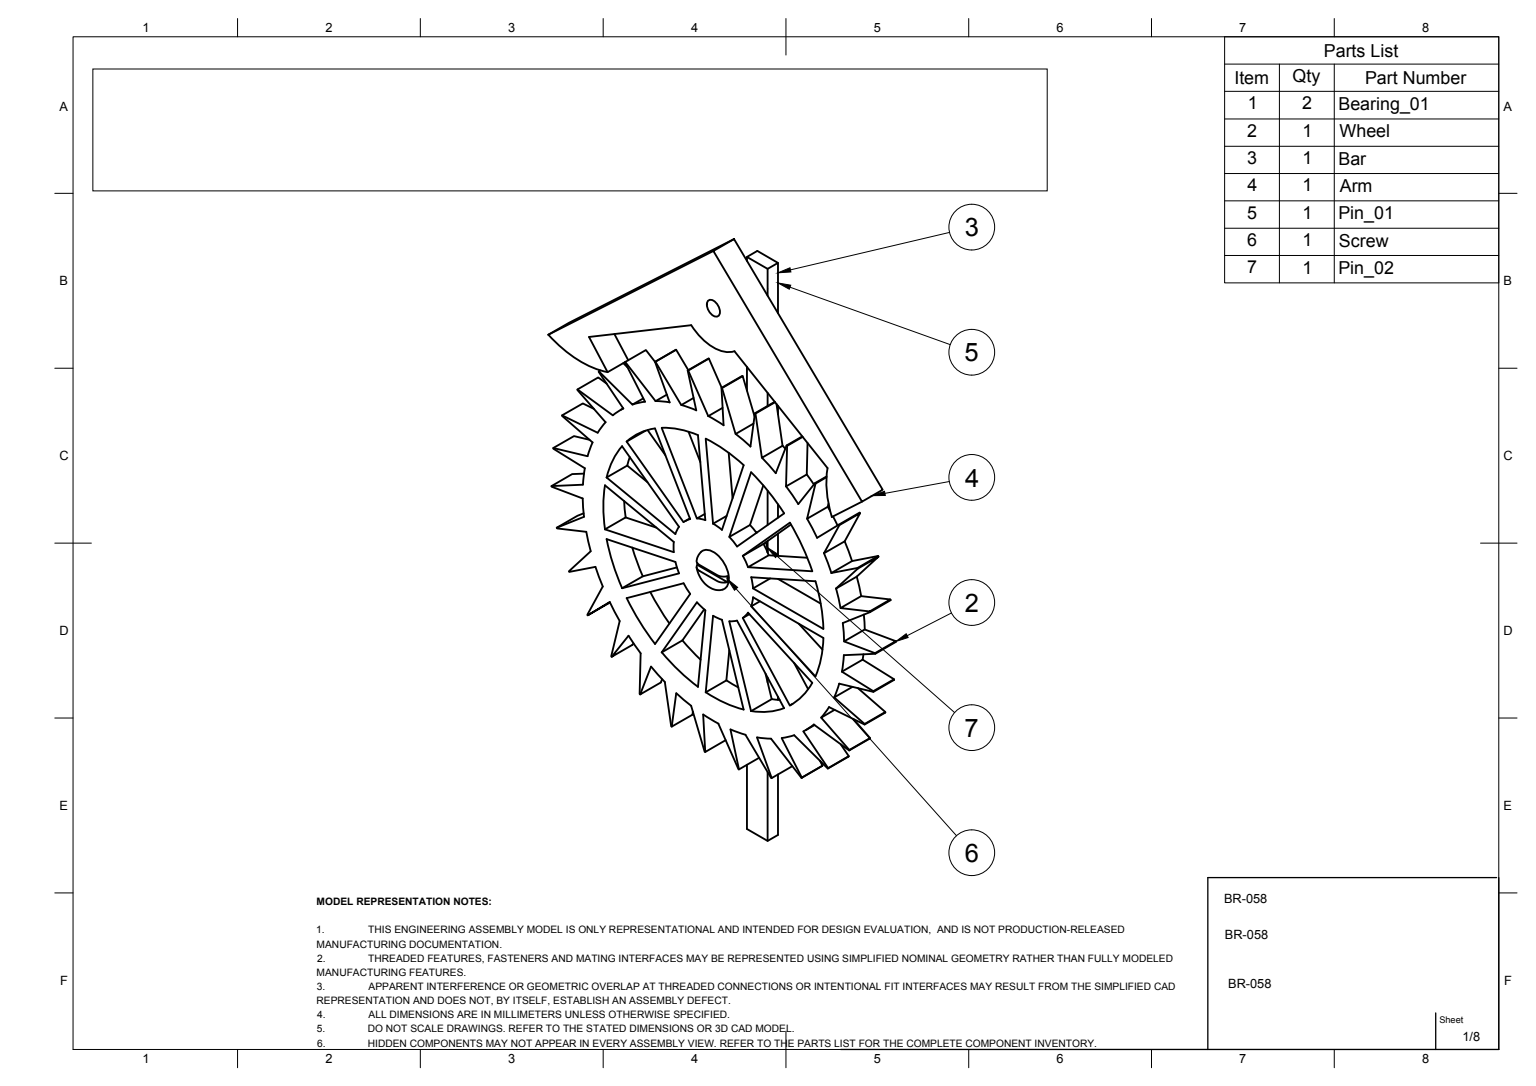
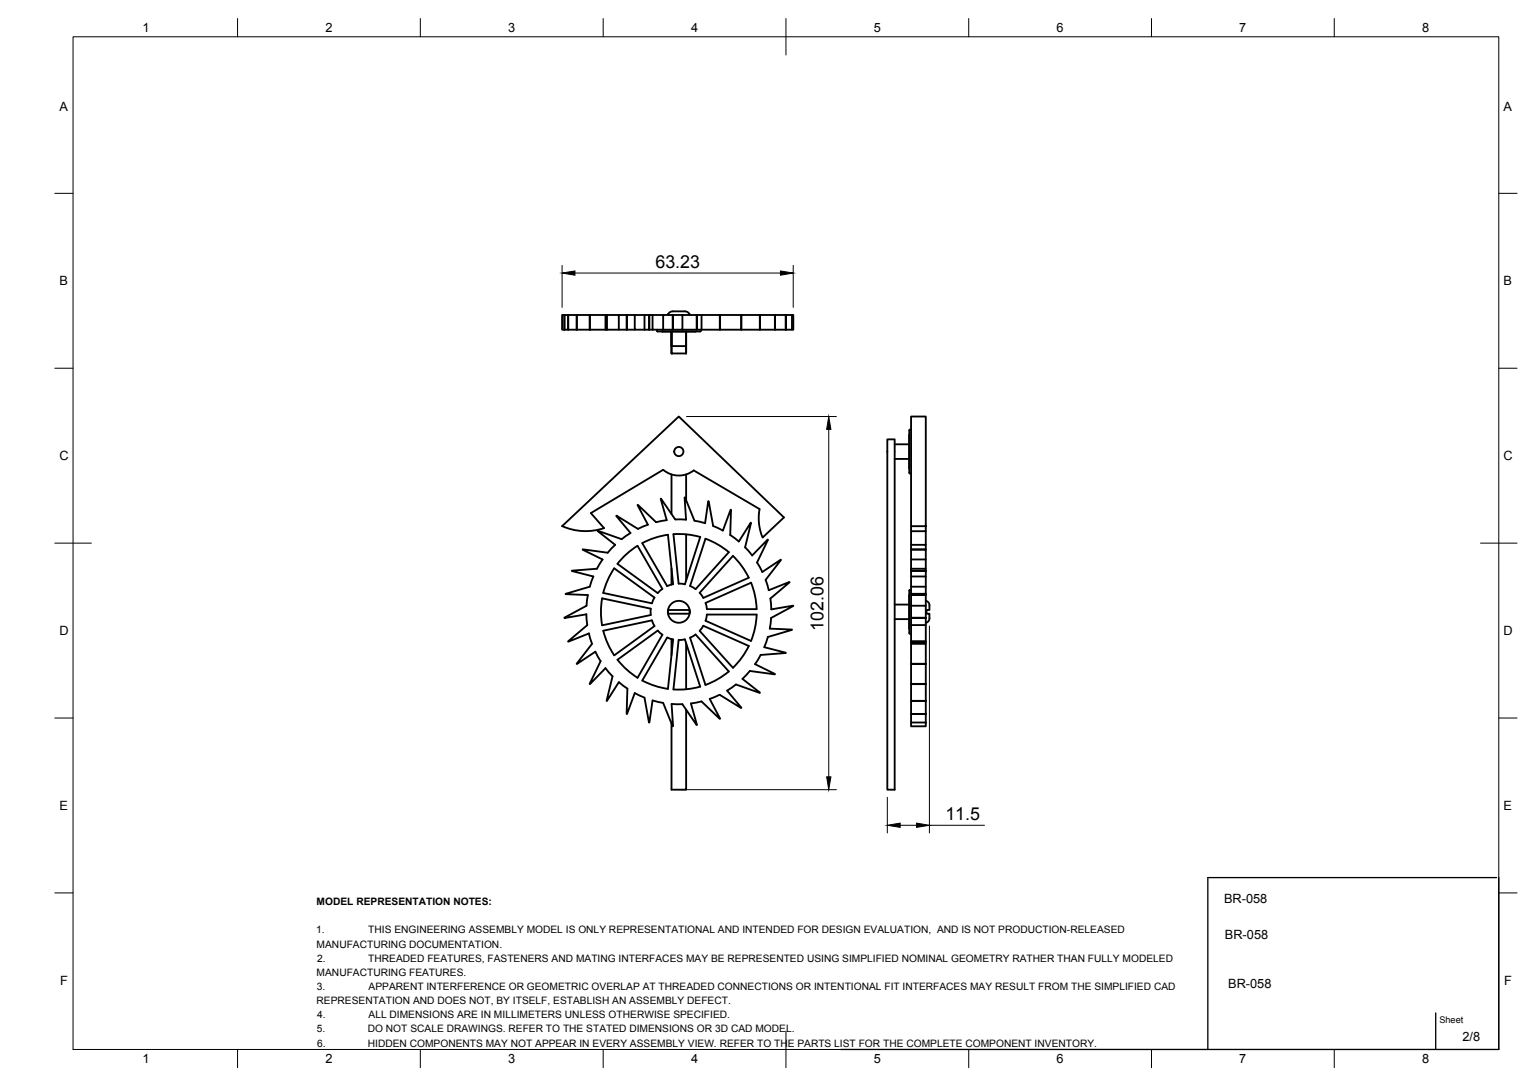
ISO-10303-21;
HEADER;
/* Generated by software containing ST-Developer
 * from STEP Tools, Inc. (www.steptools.com) 
 */

FILE_DESCRIPTION(
/* description */ (''),
/* implementation_level */ '2;1');

FILE_NAME(
/* name */ 'BR-058',
/* time_stamp */ '2026-10-12T16:07:47-07:00',
/* author */ (''),
/* organization */ (''),
/* preprocessor_version */ 'ST-DEVELOPER v20.2',
/* originating_system */ 'Autodesk Translation Framework v15.15.0.0',
/* authorisation */ '');

FILE_SCHEMA (('AUTOMOTIVE_DESIGN { 1 0 10303 214 3 1 1 }'));
ENDSEC;

DATA;
#10=MECHANICAL_DESIGN_GEOMETRIC_PRESENTATION_REPRESENTATION('',(#94,#95,
#96,#97,#98,#99,#100,#101,#102,#103),#8779);
#11=ITEM_DEFINED_TRANSFORMATION($,$,#5571,#5714);
#12=ITEM_DEFINED_TRANSFORMATION($,$,#5203,#5715);
#13=ITEM_DEFINED_TRANSFORMATION($,$,#5509,#5716);
#14=ITEM_DEFINED_TRANSFORMATION($,$,#5519,#5717);
#15=ITEM_DEFINED_TRANSFORMATION($,$,#5540,#5718);
#16=ITEM_DEFINED_TRANSFORMATION($,$,#5546,#5719);
#17=ITEM_DEFINED_TRANSFORMATION($,$,#5565,#5720);
#18=ITEM_DEFINED_TRANSFORMATION($,$,#5571,#5721);
#19=(
REPRESENTATION_RELATIONSHIP($,$,#8815,#8808)
REPRESENTATION_RELATIONSHIP_WITH_TRANSFORMATION(#11)
SHAPE_REPRESENTATION_RELATIONSHIP()
);
#20=(
REPRESENTATION_RELATIONSHIP($,$,#8809,#8808)
REPRESENTATION_RELATIONSHIP_WITH_TRANSFORMATION(#12)
SHAPE_REPRESENTATION_RELATIONSHIP()
);
#21=(
REPRESENTATION_RELATIONSHIP($,$,#8810,#8808)
REPRESENTATION_RELATIONSHIP_WITH_TRANSFORMATION(#13)
SHAPE_REPRESENTATION_RELATIONSHIP()
);
#22=(
REPRESENTATION_RELATIONSHIP($,$,#8811,#8808)
REPRESENTATION_RELATIONSHIP_WITH_TRANSFORMATION(#14)
SHAPE_REPRESENTATION_RELATIONSHIP()
);
#23=(
REPRESENTATION_RELATIONSHIP($,$,#8812,#8808)
REPRESENTATION_RELATIONSHIP_WITH_TRANSFORMATION(#15)
SHAPE_REPRESENTATION_RELATIONSHIP()
);
#24=(
REPRESENTATION_RELATIONSHIP($,$,#8813,#8808)
REPRESENTATION_RELATIONSHIP_WITH_TRANSFORMATION(#16)
SHAPE_REPRESENTATION_RELATIONSHIP()
);
#25=(
REPRESENTATION_RELATIONSHIP($,$,#8814,#8808)
REPRESENTATION_RELATIONSHIP_WITH_TRANSFORMATION(#17)
SHAPE_REPRESENTATION_RELATIONSHIP()
);
#26=(
REPRESENTATION_RELATIONSHIP($,$,#8815,#8808)
REPRESENTATION_RELATIONSHIP_WITH_TRANSFORMATION(#18)
SHAPE_REPRESENTATION_RELATIONSHIP()
);
#27=CONTEXT_DEPENDENT_SHAPE_REPRESENTATION(#19,#8800);
#28=CONTEXT_DEPENDENT_SHAPE_REPRESENTATION(#20,#8801);
#29=CONTEXT_DEPENDENT_SHAPE_REPRESENTATION(#21,#8802);
#30=CONTEXT_DEPENDENT_SHAPE_REPRESENTATION(#22,#8803);
#31=CONTEXT_DEPENDENT_SHAPE_REPRESENTATION(#23,#8804);
#32=CONTEXT_DEPENDENT_SHAPE_REPRESENTATION(#24,#8805);
#33=CONTEXT_DEPENDENT_SHAPE_REPRESENTATION(#25,#8806);
#34=CONTEXT_DEPENDENT_SHAPE_REPRESENTATION(#26,#8807);
#35=NEXT_ASSEMBLY_USAGE_OCCURRENCE('Bearing_01:1','Bearing_01:1',
'Bearing_01:1',#8817,#8824,'Bearing_01:1');
#36=NEXT_ASSEMBLY_USAGE_OCCURRENCE('Wheel:1','Wheel:1','Wheel:1',#8817,
#8818,'Wheel:1');
#37=NEXT_ASSEMBLY_USAGE_OCCURRENCE('Bar:1','Bar:1','Bar:1',#8817,#8819,
'Bar:1');
#38=NEXT_ASSEMBLY_USAGE_OCCURRENCE('Arm:1','Arm:1','Arm:1',#8817,#8820,
'Arm:1');
#39=NEXT_ASSEMBLY_USAGE_OCCURRENCE('Pin_01:1','Pin_01:1','Pin_01:1',#8817,
#8821,'Pin_01:1');
#40=NEXT_ASSEMBLY_USAGE_OCCURRENCE('Screw:1','Screw:1','Screw:1',#8817,
#8822,'Screw:1');
#41=NEXT_ASSEMBLY_USAGE_OCCURRENCE('Pin_02:1','Pin_02:1','Pin_02:1',#8817,
#8823,'Pin_02:1');
#42=NEXT_ASSEMBLY_USAGE_OCCURRENCE('Bearing_01:2','Bearing_01:2',
'Bearing_01:2',#8817,#8824,'Bearing_01:2');
#43=CONICAL_SURFACE('',#5582,4.8,0.785398163397444);
#44=CONICAL_SURFACE('',#5593,4.845,0.785398163397444);
#45=CONICAL_SURFACE('',#5599,3.1184375,0.785398163397448);
#46=CONICAL_SURFACE('',#5617,3.0734375,0.785398163397448);
#47=CONICAL_SURFACE('',#5639,4.36638040039984,0.52359877559829);
#48=CONICAL_SURFACE('',#5648,4.57071796769724,1.04719755119659);
#49=CONICAL_SURFACE('',#5657,4.62071796769724,1.04719755119659);
#50=CONICAL_SURFACE('',#5666,4.27977786002139,0.52359877559829);
#51=CONICAL_SURFACE('',#5680,4.36638040039984,0.52359877559829);
#52=CONICAL_SURFACE('',#5689,4.57071796769724,1.04719755119659);
#53=CONICAL_SURFACE('',#5698,4.62071796769724,1.04719755119659);
#54=CONICAL_SURFACE('',#5707,4.27977786002139,0.52359877559829);
#55=TOROIDAL_SURFACE('',#5558,1.77525512860841,1.25);
#56=TOROIDAL_SURFACE('',#5584,5.8,0.2);
#57=TOROIDAL_SURFACE('',#5590,5.8,0.2);
#58=TOROIDAL_SURFACE('',#5605,3.25741379310345,0.138976293103448);
#59=TOROIDAL_SURFACE('',#5611,3.25741379310345,0.138976293103448);
#60=TOROIDAL_SURFACE('',#5619,2.2,0.2);
#61=TOROIDAL_SURFACE('',#5625,2.2,0.2);
#62=TOROIDAL_SURFACE('',#5635,4.14313829631318,0.0900000000000005);
#63=TOROIDAL_SURFACE('',#5641,4.38370090847553,0.0200000000000002);
#64=TOROIDAL_SURFACE('',#5644,4.58,0.119999999999999);
#65=TOROIDAL_SURFACE('',#5650,4.51071796769724,0.12);
#66=TOROIDAL_SURFACE('',#5653,4.51071796769724,0.22);
#67=TOROIDAL_SURFACE('',#5659,4.58,0.219999999999999);
#68=TOROIDAL_SURFACE('',#5662,4.38370090847553,0.12);
#69=TOROIDAL_SURFACE('',#5676,4.14313829631318,0.0900000000000005);
#70=TOROIDAL_SURFACE('',#5682,4.38370090847553,0.0200000000000002);
#71=TOROIDAL_SURFACE('',#5685,4.58,0.119999999999999);
#72=TOROIDAL_SURFACE('',#5691,4.51071796769724,0.12);
#73=TOROIDAL_SURFACE('',#5694,4.51071796769724,0.22);
#74=TOROIDAL_SURFACE('',#5700,4.58,0.219999999999999);
#75=TOROIDAL_SURFACE('',#5703,4.38370090847553,0.12);
#76=B_SPLINE_CURVE_WITH_KNOTS('',3,(#8451,#8452,#8453,#8454,#8455,#8456,
#8457,#8458,#8459,#8460),.UNSPECIFIED.,.F.,.F.,(4,2,2,2,4),(0.042485066523561,
0.0459790210316649,0.0922828710125633,0.139235462221755,0.187535404261205),
 .UNSPECIFIED.);
#77=B_SPLINE_CURVE_WITH_KNOTS('',3,(#8464,#8465,#8466,#8467,#8468,#8469,
#8470,#8471,#8472,#8473),.UNSPECIFIED.,.F.,.F.,(4,2,2,2,4),(0.589058059380764,
0.637358001420214,0.684310592629405,0.730614442610304,0.734108397118407),
 .UNSPECIFIED.);
#78=B_SPLINE_CURVE_WITH_KNOTS('',3,(#8485,#8486,#8487,#8488,#8489,#8490,
#8491,#8492,#8493,#8494),.UNSPECIFIED.,.F.,.F.,(4,2,2,2,4),(0.589058059380764,
0.637358001420214,0.684310592629405,0.730614442610304,0.734108397118408),
 .UNSPECIFIED.);
#79=B_SPLINE_CURVE_WITH_KNOTS('',3,(#8497,#8498,#8499,#8500,#8501,#8502,
#8503,#8504,#8505,#8506),.UNSPECIFIED.,.F.,.F.,(4,2,2,2,4),(0.0424850665235609,
0.0459790210316651,0.0922828710125635,0.139235462221755,0.187535404261205),
 .UNSPECIFIED.);
#80=SHAPE_REPRESENTATION_RELATIONSHIP('SRR','None',#8809,#87);
#81=SHAPE_REPRESENTATION_RELATIONSHIP('SRR','None',#8810,#88);
#82=SHAPE_REPRESENTATION_RELATIONSHIP('SRR','None',#8811,#89);
#83=SHAPE_REPRESENTATION_RELATIONSHIP('SRR','None',#8812,#90);
#84=SHAPE_REPRESENTATION_RELATIONSHIP('SRR','None',#8813,#91);
#85=SHAPE_REPRESENTATION_RELATIONSHIP('SRR','None',#8814,#92);
#86=SHAPE_REPRESENTATION_RELATIONSHIP('SRR','None',#8815,#93);
#87=ADVANCED_BREP_SHAPE_REPRESENTATION('',(#104),#8772);
#88=ADVANCED_BREP_SHAPE_REPRESENTATION('',(#105),#8773);
#89=ADVANCED_BREP_SHAPE_REPRESENTATION('',(#106),#8774);
#90=ADVANCED_BREP_SHAPE_REPRESENTATION('',(#107),#8775);
#91=ADVANCED_BREP_SHAPE_REPRESENTATION('',(#108),#8776);
#92=ADVANCED_BREP_SHAPE_REPRESENTATION('',(#109),#8777);
#93=ADVANCED_BREP_SHAPE_REPRESENTATION('',(#110,#111,#112,#113),#8778);
#94=STYLED_ITEM('',(#8853),#104);
#95=STYLED_ITEM('',(#8854),#105);
#96=STYLED_ITEM('',(#8855),#106);
#97=STYLED_ITEM('',(#8854),#107);
#98=STYLED_ITEM('',(#8856),#108);
#99=STYLED_ITEM('',(#8856),#109);
#100=STYLED_ITEM('',(#8856),#110);
#101=STYLED_ITEM('',(#8856),#111);
#102=STYLED_ITEM('',(#8856),#112);
#103=STYLED_ITEM('',(#8856),#113);
#104=MANIFOLD_SOLID_BREP('Body1',#5114);
#105=MANIFOLD_SOLID_BREP('Body1',#5115);
#106=MANIFOLD_SOLID_BREP('Body1',#5116);
#107=MANIFOLD_SOLID_BREP('Body1',#5117);
#108=MANIFOLD_SOLID_BREP('Body1',#5118);
#109=MANIFOLD_SOLID_BREP('Body1',#5119);
#110=MANIFOLD_SOLID_BREP('Body1',#5120);
#111=MANIFOLD_SOLID_BREP('Body2',#5121);
#112=MANIFOLD_SOLID_BREP('Body3',#5122);
#113=MANIFOLD_SOLID_BREP('Body4',#5123);
#114=FACE_BOUND('',#934,.T.);
#115=FACE_BOUND('',#935,.T.);
#116=FACE_BOUND('',#936,.T.);
#117=FACE_BOUND('',#937,.T.);
#118=FACE_BOUND('',#938,.T.);
#119=FACE_BOUND('',#939,.T.);
#120=FACE_BOUND('',#940,.T.);
#121=FACE_BOUND('',#941,.T.);
#122=FACE_BOUND('',#942,.T.);
#123=FACE_BOUND('',#943,.T.);
#124=FACE_BOUND('',#944,.T.);
#125=FACE_BOUND('',#945,.T.);
#126=FACE_BOUND('',#946,.T.);
#127=FACE_BOUND('',#947,.T.);
#128=FACE_BOUND('',#948,.T.);
#129=FACE_BOUND('',#949,.T.);
#130=FACE_BOUND('',#951,.T.);
#131=FACE_BOUND('',#952,.T.);
#132=FACE_BOUND('',#953,.T.);
#133=FACE_BOUND('',#954,.T.);
#134=FACE_BOUND('',#955,.T.);
#135=FACE_BOUND('',#956,.T.);
#136=FACE_BOUND('',#957,.T.);
#137=FACE_BOUND('',#958,.T.);
#138=FACE_BOUND('',#959,.T.);
#139=FACE_BOUND('',#960,.T.);
#140=FACE_BOUND('',#961,.T.);
#141=FACE_BOUND('',#962,.T.);
#142=FACE_BOUND('',#963,.T.);
#143=FACE_BOUND('',#964,.T.);
#144=FACE_BOUND('',#965,.T.);
#145=FACE_BOUND('',#966,.T.);
#146=FACE_BOUND('',#973,.T.);
#147=FACE_BOUND('',#975,.T.);
#148=FACE_BOUND('',#987,.T.);
#149=FACE_BOUND('',#989,.T.);
#150=FACE_BOUND('',#994,.T.);
#151=FACE_BOUND('',#1015,.T.);
#152=FACE_BOUND('',#1017,.T.);
#153=FACE_BOUND('',#1019,.T.);
#154=FACE_BOUND('',#1021,.T.);
#155=FACE_BOUND('',#1033,.T.);
#156=FACE_BOUND('',#1035,.T.);
#157=FACE_BOUND('',#1037,.T.);
#158=FACE_BOUND('',#1039,.T.);
#159=FACE_BOUND('',#1053,.T.);
#160=FACE_BOUND('',#1055,.T.);
#161=FACE_BOUND('',#1057,.T.);
#162=FACE_BOUND('',#1059,.T.);
#163=FACE_BOUND('',#1061,.T.);
#164=FACE_BOUND('',#1075,.T.);
#165=FACE_BOUND('',#1077,.T.);
#166=FACE_BOUND('',#1079,.T.);
#167=FACE_BOUND('',#1081,.T.);
#168=FACE_BOUND('',#1083,.T.);
#169=CIRCLE('',#5208,25.2882678496568);
#170=CIRCLE('',#5209,25.2882678496568);
#171=CIRCLE('',#5211,25.2882678496568);
#172=CIRCLE('',#5212,25.2882678496568);
#173=CIRCLE('',#5217,25.2882678496568);
#174=CIRCLE('',#5218,25.2882678496568);
#175=CIRCLE('',#5220,25.2882678496568);
#176=CIRCLE('',#5221,25.2882678496568);
#177=CIRCLE('',#5226,25.2882678496568);
#178=CIRCLE('',#5227,25.2882678496568);
#179=CIRCLE('',#5232,25.2882678496568);
#180=CIRCLE('',#5233,25.2882678496568);
#181=CIRCLE('',#5235,25.2882678496568);
#182=CIRCLE('',#5236,25.2882678496568);
#183=CIRCLE('',#5244,25.2882678496568);
#184=CIRCLE('',#5245,25.2882678496568);
#185=CIRCLE('',#5250,25.2882678496568);
#186=CIRCLE('',#5251,25.2882678496568);
#187=CIRCLE('',#5258,21.2882678496568);
#188=CIRCLE('',#5259,21.2882678496568);
#189=CIRCLE('',#5261,21.2882678496568);
#190=CIRCLE('',#5262,21.2882678496568);
#191=CIRCLE('',#5264,7.71108476483471);
#192=CIRCLE('',#5265,7.71108476483471);
#193=CIRCLE('',#5267,7.71108476483471);
#194=CIRCLE('',#5268,7.71108476483471);
#195=CIRCLE('',#5272,21.2882678496568);
#196=CIRCLE('',#5273,21.2882678496568);
#197=CIRCLE('',#5275,7.71108476483471);
#198=CIRCLE('',#5276,7.71108476483471);
#199=CIRCLE('',#5280,21.2882678496568);
#200=CIRCLE('',#5281,21.2882678496568);
#201=CIRCLE('',#5283,7.71108476483471);
#202=CIRCLE('',#5284,7.71108476483471);
#203=CIRCLE('',#5289,25.2882678496568);
#204=CIRCLE('',#5290,25.2882678496568);
#205=CIRCLE('',#5292,25.2882678496568);
#206=CIRCLE('',#5293,25.2882678496568);
#207=CIRCLE('',#5298,25.2882678496568);
#208=CIRCLE('',#5299,25.2882678496568);
#209=CIRCLE('',#5301,25.2882678496568);
#210=CIRCLE('',#5302,25.2882678496568);
#211=CIRCLE('',#5307,25.2882678496568);
#212=CIRCLE('',#5308,25.2882678496568);
#213=CIRCLE('',#5316,25.2882678496568);
#214=CIRCLE('',#5317,25.2882678496568);
#215=CIRCLE('',#5324,21.2882678496568);
#216=CIRCLE('',#5325,21.2882678496568);
#217=CIRCLE('',#5327,21.2882678496568);
#218=CIRCLE('',#5328,21.2882678496568);
#219=CIRCLE('',#5330,7.71108476483471);
#220=CIRCLE('',#5331,7.71108476483471);
#221=CIRCLE('',#5333,7.71108476483471);
#222=CIRCLE('',#5334,7.71108476483471);
#223=CIRCLE('',#5338,21.2882678496568);
#224=CIRCLE('',#5339,21.2882678496568);
#225=CIRCLE('',#5341,7.71108476483471);
#226=CIRCLE('',#5342,7.71108476483471);
#227=CIRCLE('',#5346,21.2882678496568);
#228=CIRCLE('',#5347,21.2882678496568);
#229=CIRCLE('',#5349,21.2882678496568);
#230=CIRCLE('',#5350,21.2882678496568);
#231=CIRCLE('',#5352,7.71108476483471);
#232=CIRCLE('',#5353,7.71108476483471);
#233=CIRCLE('',#5355,7.71108476483471);
#234=CIRCLE('',#5356,7.71108476483471);
#235=CIRCLE('',#5360,21.2882678496568);
#236=CIRCLE('',#5361,21.2882678496568);
#237=CIRCLE('',#5363,21.2882678496568);
#238=CIRCLE('',#5364,21.2882678496568);
#239=CIRCLE('',#5366,7.71108476483471);
#240=CIRCLE('',#5367,7.71108476483471);
#241=CIRCLE('',#5369,7.71108476483471);
#242=CIRCLE('',#5370,7.71108476483471);
#243=CIRCLE('',#5374,21.2882678496568);
#244=CIRCLE('',#5375,21.2882678496568);
#245=CIRCLE('',#5377,7.71108476483471);
#246=CIRCLE('',#5378,7.71108476483471);
#247=CIRCLE('',#5384,21.2882678496568);
#248=CIRCLE('',#5385,21.2882678496568);
#249=CIRCLE('',#5387,7.71108476483471);
#250=CIRCLE('',#5388,7.71108476483471);
#251=CIRCLE('',#5395,25.2882678496568);
#252=CIRCLE('',#5396,25.2882678496568);
#253=CIRCLE('',#5398,25.2882678496568);
#254=CIRCLE('',#5399,25.2882678496568);
#255=CIRCLE('',#5404,25.2882678496568);
#256=CIRCLE('',#5405,25.2882678496568);
#257=CIRCLE('',#5410,25.2882678496568);
#258=CIRCLE('',#5411,25.2882678496568);
#259=CIRCLE('',#5413,25.2882678496568);
#260=CIRCLE('',#5414,25.2882678496568);
#261=CIRCLE('',#5419,25.2882678496568);
#262=CIRCLE('',#5420,25.2882678496568);
#263=CIRCLE('',#5422,25.2882678496568);
#264=CIRCLE('',#5423,25.2882678496568);
#265=CIRCLE('',#5437,25.2882678496568);
#266=CIRCLE('',#5438,25.2882678496568);
#267=CIRCLE('',#5442,21.2882678496568);
#268=CIRCLE('',#5443,21.2882678496568);
#269=CIRCLE('',#5445,7.71108476483471);
#270=CIRCLE('',#5446,7.71108476483471);
#271=CIRCLE('',#5450,21.2882678496568);
#272=CIRCLE('',#5451,21.2882678496568);
#273=CIRCLE('',#5453,7.71108476483471);
#274=CIRCLE('',#5454,7.71108476483471);
#275=CIRCLE('',#5461,25.2882678496568);
#276=CIRCLE('',#5462,25.2882678496568);
#277=CIRCLE('',#5464,25.2882678496568);
#278=CIRCLE('',#5465,25.2882678496568);
#279=CIRCLE('',#5470,25.2882678496568);
#280=CIRCLE('',#5471,25.2882678496568);
#281=CIRCLE('',#5476,25.2882678496568);
#282=CIRCLE('',#5477,25.2882678496568);
#283=CIRCLE('',#5479,25.2882678496568);
#284=CIRCLE('',#5480,25.2882678496568);
#285=CIRCLE('',#5485,25.2882678496568);
#286=CIRCLE('',#5486,25.2882678496568);
#287=CIRCLE('',#5491,25.2882678496568);
#288=CIRCLE('',#5492,25.2882678496568);
#289=CIRCLE('',#5505,1.99137169252308);
#290=CIRCLE('',#5506,1.99137169252308);
#291=CIRCLE('',#5511,1.26938918348039);
#292=CIRCLE('',#5512,1.26938918348039);
#293=CIRCLE('',#5523,6.58030196793658);
#294=CIRCLE('',#5524,6.58030196793658);
#295=CIRCLE('',#5528,1.26938918348039);
#296=CIRCLE('',#5529,1.26938918348039);
#297=CIRCLE('',#5532,13.6540067108022);
#298=CIRCLE('',#5533,13.6540067108022);
#299=CIRCLE('',#5536,15.694333954976);
#300=CIRCLE('',#5537,15.694333954976);
#301=CIRCLE('',#5542,2.00038918348039);
#302=CIRCLE('',#5543,2.00038918348039);
#303=CIRCLE('',#5548,3.);
#304=CIRCLE('',#5549,1.99137169252308);
#305=CIRCLE('',#5552,2.94442677252053);
#306=CIRCLE('',#5553,2.94442677252053);
#307=CIRCLE('',#5554,2.94442677252053);
#308=CIRCLE('',#5557,1.77525512860841);
#309=CIRCLE('',#5559,1.25);
#310=CIRCLE('',#5560,1.77525512860841);
#311=CIRCLE('',#5563,1.99137169252308);
#312=CIRCLE('',#5567,1.99137169252308);
#313=CIRCLE('',#5568,1.99137169252308);
#314=CIRCLE('',#5573,4.8);
#315=CIRCLE('',#5574,4.8);
#316=CIRCLE('',#5576,4.872);
#317=CIRCLE('',#5577,4.872);
#318=CIRCLE('',#5579,4.8);
#319=CIRCLE('',#5580,4.8);
#320=CIRCLE('',#5581,4.8);
#321=CIRCLE('',#5583,4.845);
#322=CIRCLE('',#5585,6.);
#323=CIRCLE('',#5586,0.2);
#324=CIRCLE('',#5587,5.8);
#325=CIRCLE('',#5589,6.);
#326=CIRCLE('',#5591,5.8);
#327=CIRCLE('',#5592,0.2);
#328=CIRCLE('',#5594,4.845);
#329=CIRCLE('',#5600,3.1184375);
#330=CIRCLE('',#5601,3.0734375);
#331=CIRCLE('',#5602,3.1184375);
#332=CIRCLE('',#5604,3.1184375);
#333=CIRCLE('',#5606,0.138976293103448);
#334=CIRCLE('',#5607,3.2);
#335=CIRCLE('',#5609,3.272);
#336=CIRCLE('',#5610,3.272);
#337=CIRCLE('',#5612,3.2);
#338=CIRCLE('',#5613,0.138976293103448);
#339=CIRCLE('',#5614,3.1184375);
#340=CIRCLE('',#5616,3.1184375);
#341=CIRCLE('',#5618,3.0734375);
#342=CIRCLE('',#5620,2.2);
#343=CIRCLE('',#5621,0.2);
#344=CIRCLE('',#5622,2.);
#345=CIRCLE('',#5624,2.);
#346=CIRCLE('',#5626,0.2);
#347=CIRCLE('',#5627,2.2);
#348=CIRCLE('',#5633,3.2);
#349=CIRCLE('',#5634,3.2);
#350=CIRCLE('',#5636,4.22108058265378);
#351=CIRCLE('',#5637,0.0900000000000005);
#352=CIRCLE('',#5638,4.14313829631318);
#353=CIRCLE('',#5640,4.36638040039984);
#354=CIRCLE('',#5642,4.38370090847553);
#355=CIRCLE('',#5643,0.0200000000000002);
#356=CIRCLE('',#5645,4.64);
#357=CIRCLE('',#5646,0.119999999999999);
#358=CIRCLE('',#5647,4.58);
#359=CIRCLE('',#5649,4.57071796769724);
#360=CIRCLE('',#5651,4.39071796769724);
#361=CIRCLE('',#5652,0.12);
#362=CIRCLE('',#5654,4.62071796769724);
#363=CIRCLE('',#5655,0.22);
#364=CIRCLE('',#5656,4.29071796769724);
#365=CIRCLE('',#5658,4.69);
#366=CIRCLE('',#5660,4.58);
#367=CIRCLE('',#5661,0.219999999999999);
#368=CIRCLE('',#5663,4.27977786002139);
#369=CIRCLE('',#5664,0.12);
#370=CIRCLE('',#5665,4.38370090847553);
#371=CIRCLE('',#5667,4.13736479362129);
#372=CIRCLE('',#5674,3.2);
#373=CIRCLE('',#5675,3.2);
#374=CIRCLE('',#5677,4.22108058265378);
#375=CIRCLE('',#5678,0.0900000000000005);
#376=CIRCLE('',#5679,4.14313829631318);
#377=CIRCLE('',#5681,4.36638040039984);
#378=CIRCLE('',#5683,4.38370090847553);
#379=CIRCLE('',#5684,0.0200000000000002);
#380=CIRCLE('',#5686,4.64);
#381=CIRCLE('',#5687,0.119999999999999);
#382=CIRCLE('',#5688,4.58);
#383=CIRCLE('',#5690,4.57071796769724);
#384=CIRCLE('',#5692,4.39071796769724);
#385=CIRCLE('',#5693,0.12);
#386=CIRCLE('',#5695,4.62071796769724);
#387=CIRCLE('',#5696,0.22);
#388=CIRCLE('',#5697,4.29071796769724);
#389=CIRCLE('',#5699,4.69);
#390=CIRCLE('',#5701,4.58);
#391=CIRCLE('',#5702,0.219999999999999);
#392=CIRCLE('',#5704,4.27977786002139);
#393=CIRCLE('',#5705,0.12);
#394=CIRCLE('',#5706,4.38370090847553);
#395=CIRCLE('',#5708,4.13736479362129);
#396=CYLINDRICAL_SURFACE('',#5207,25.2882678496568);
#397=CYLINDRICAL_SURFACE('',#5210,25.2882678496568);
#398=CYLINDRICAL_SURFACE('',#5216,25.2882678496568);
#399=CYLINDRICAL_SURFACE('',#5219,25.2882678496568);
#400=CYLINDRICAL_SURFACE('',#5225,25.2882678496568);
#401=CYLINDRICAL_SURFACE('',#5231,25.2882678496568);
#402=CYLINDRICAL_SURFACE('',#5234,25.2882678496568);
#403=CYLINDRICAL_SURFACE('',#5243,25.2882678496568);
#404=CYLINDRICAL_SURFACE('',#5249,25.2882678496568);
#405=CYLINDRICAL_SURFACE('',#5257,21.2882678496568);
#406=CYLINDRICAL_SURFACE('',#5260,21.2882678496568);
#407=CYLINDRICAL_SURFACE('',#5263,7.71108476483471);
#408=CYLINDRICAL_SURFACE('',#5266,7.71108476483471);
#409=CYLINDRICAL_SURFACE('',#5271,21.2882678496568);
#410=CYLINDRICAL_SURFACE('',#5274,7.71108476483471);
#411=CYLINDRICAL_SURFACE('',#5279,21.2882678496568);
#412=CYLINDRICAL_SURFACE('',#5282,7.71108476483471);
#413=CYLINDRICAL_SURFACE('',#5288,25.2882678496568);
#414=CYLINDRICAL_SURFACE('',#5291,25.2882678496568);
#415=CYLINDRICAL_SURFACE('',#5297,25.2882678496568);
#416=CYLINDRICAL_SURFACE('',#5300,25.2882678496568);
#417=CYLINDRICAL_SURFACE('',#5306,25.2882678496568);
#418=CYLINDRICAL_SURFACE('',#5315,25.2882678496568);
#419=CYLINDRICAL_SURFACE('',#5323,21.2882678496568);
#420=CYLINDRICAL_SURFACE('',#5326,21.2882678496568);
#421=CYLINDRICAL_SURFACE('',#5329,7.71108476483471);
#422=CYLINDRICAL_SURFACE('',#5332,7.71108476483471);
#423=CYLINDRICAL_SURFACE('',#5337,21.2882678496568);
#424=CYLINDRICAL_SURFACE('',#5340,7.71108476483471);
#425=CYLINDRICAL_SURFACE('',#5345,21.2882678496568);
#426=CYLINDRICAL_SURFACE('',#5348,21.2882678496568);
#427=CYLINDRICAL_SURFACE('',#5351,7.71108476483471);
#428=CYLINDRICAL_SURFACE('',#5354,7.71108476483471);
#429=CYLINDRICAL_SURFACE('',#5359,21.2882678496568);
#430=CYLINDRICAL_SURFACE('',#5362,21.2882678496568);
#431=CYLINDRICAL_SURFACE('',#5365,7.71108476483471);
#432=CYLINDRICAL_SURFACE('',#5368,7.71108476483471);
#433=CYLINDRICAL_SURFACE('',#5373,21.2882678496568);
#434=CYLINDRICAL_SURFACE('',#5376,7.71108476483471);
#435=CYLINDRICAL_SURFACE('',#5383,21.2882678496568);
#436=CYLINDRICAL_SURFACE('',#5386,7.71108476483471);
#437=CYLINDRICAL_SURFACE('',#5394,25.2882678496568);
#438=CYLINDRICAL_SURFACE('',#5397,25.2882678496568);
#439=CYLINDRICAL_SURFACE('',#5403,25.2882678496568);
#440=CYLINDRICAL_SURFACE('',#5409,25.2882678496568);
#441=CYLINDRICAL_SURFACE('',#5412,25.2882678496568);
#442=CYLINDRICAL_SURFACE('',#5418,25.2882678496568);
#443=CYLINDRICAL_SURFACE('',#5421,25.2882678496568);
#444=CYLINDRICAL_SURFACE('',#5436,25.2882678496568);
#445=CYLINDRICAL_SURFACE('',#5441,21.2882678496568);
#446=CYLINDRICAL_SURFACE('',#5444,7.71108476483471);
#447=CYLINDRICAL_SURFACE('',#5449,21.2882678496568);
#448=CYLINDRICAL_SURFACE('',#5452,7.71108476483471);
#449=CYLINDRICAL_SURFACE('',#5460,25.2882678496568);
#450=CYLINDRICAL_SURFACE('',#5463,25.2882678496568);
#451=CYLINDRICAL_SURFACE('',#5469,25.2882678496568);
#452=CYLINDRICAL_SURFACE('',#5475,25.2882678496568);
#453=CYLINDRICAL_SURFACE('',#5478,25.2882678496568);
#454=CYLINDRICAL_SURFACE('',#5484,25.2882678496568);
#455=CYLINDRICAL_SURFACE('',#5490,25.2882678496568);
#456=CYLINDRICAL_SURFACE('',#5504,1.99137169252308);
#457=CYLINDRICAL_SURFACE('',#5510,1.26938918348039);
#458=CYLINDRICAL_SURFACE('',#5522,6.58030196793658);
#459=CYLINDRICAL_SURFACE('',#5527,1.26938918348039);
#460=CYLINDRICAL_SURFACE('',#5531,13.6540067108022);
#461=CYLINDRICAL_SURFACE('',#5535,15.694333954976);
#462=CYLINDRICAL_SURFACE('',#5541,2.00038918348039);
#463=CYLINDRICAL_SURFACE('',#5564,1.99137169252308);
#464=CYLINDRICAL_SURFACE('',#5566,1.99137169252308);
#465=CYLINDRICAL_SURFACE('',#5572,4.8);
#466=CYLINDRICAL_SURFACE('',#5575,4.872);
#467=CYLINDRICAL_SURFACE('',#5578,4.8);
#468=CYLINDRICAL_SURFACE('',#5588,6.);
#469=CYLINDRICAL_SURFACE('',#5603,3.1184375);
#470=CYLINDRICAL_SURFACE('',#5608,3.272);
#471=CYLINDRICAL_SURFACE('',#5615,3.1184375);
#472=CYLINDRICAL_SURFACE('',#5623,2.);
#473=CYLINDRICAL_SURFACE('',#5632,3.2);
#474=CYLINDRICAL_SURFACE('',#5673,3.2);
#475=FACE_OUTER_BOUND('',#752,.T.);
#476=FACE_OUTER_BOUND('',#753,.T.);
#477=FACE_OUTER_BOUND('',#754,.T.);
#478=FACE_OUTER_BOUND('',#755,.T.);
#479=FACE_OUTER_BOUND('',#756,.T.);
#480=FACE_OUTER_BOUND('',#757,.T.);
#481=FACE_OUTER_BOUND('',#758,.T.);
#482=FACE_OUTER_BOUND('',#759,.T.);
#483=FACE_OUTER_BOUND('',#760,.T.);
#484=FACE_OUTER_BOUND('',#761,.T.);
#485=FACE_OUTER_BOUND('',#762,.T.);
#486=FACE_OUTER_BOUND('',#763,.T.);
#487=FACE_OUTER_BOUND('',#764,.T.);
#488=FACE_OUTER_BOUND('',#765,.T.);
#489=FACE_OUTER_BOUND('',#766,.T.);
#490=FACE_OUTER_BOUND('',#767,.T.);
#491=FACE_OUTER_BOUND('',#768,.T.);
#492=FACE_OUTER_BOUND('',#769,.T.);
#493=FACE_OUTER_BOUND('',#770,.T.);
#494=FACE_OUTER_BOUND('',#771,.T.);
#495=FACE_OUTER_BOUND('',#772,.T.);
#496=FACE_OUTER_BOUND('',#773,.T.);
#497=FACE_OUTER_BOUND('',#774,.T.);
#498=FACE_OUTER_BOUND('',#775,.T.);
#499=FACE_OUTER_BOUND('',#776,.T.);
#500=FACE_OUTER_BOUND('',#777,.T.);
#501=FACE_OUTER_BOUND('',#778,.T.);
#502=FACE_OUTER_BOUND('',#779,.T.);
#503=FACE_OUTER_BOUND('',#780,.T.);
#504=FACE_OUTER_BOUND('',#781,.T.);
#505=FACE_OUTER_BOUND('',#782,.T.);
#506=FACE_OUTER_BOUND('',#783,.T.);
#507=FACE_OUTER_BOUND('',#784,.T.);
#508=FACE_OUTER_BOUND('',#785,.T.);
#509=FACE_OUTER_BOUND('',#786,.T.);
#510=FACE_OUTER_BOUND('',#787,.T.);
#511=FACE_OUTER_BOUND('',#788,.T.);
#512=FACE_OUTER_BOUND('',#789,.T.);
#513=FACE_OUTER_BOUND('',#790,.T.);
#514=FACE_OUTER_BOUND('',#791,.T.);
#515=FACE_OUTER_BOUND('',#792,.T.);
#516=FACE_OUTER_BOUND('',#793,.T.);
#517=FACE_OUTER_BOUND('',#794,.T.);
#518=FACE_OUTER_BOUND('',#795,.T.);
#519=FACE_OUTER_BOUND('',#796,.T.);
#520=FACE_OUTER_BOUND('',#797,.T.);
#521=FACE_OUTER_BOUND('',#798,.T.);
#522=FACE_OUTER_BOUND('',#799,.T.);
#523=FACE_OUTER_BOUND('',#800,.T.);
#524=FACE_OUTER_BOUND('',#801,.T.);
#525=FACE_OUTER_BOUND('',#802,.T.);
#526=FACE_OUTER_BOUND('',#803,.T.);
#527=FACE_OUTER_BOUND('',#804,.T.);
#528=FACE_OUTER_BOUND('',#805,.T.);
#529=FACE_OUTER_BOUND('',#806,.T.);
#530=FACE_OUTER_BOUND('',#807,.T.);
#531=FACE_OUTER_BOUND('',#808,.T.);
#532=FACE_OUTER_BOUND('',#809,.T.);
#533=FACE_OUTER_BOUND('',#810,.T.);
#534=FACE_OUTER_BOUND('',#811,.T.);
#535=FACE_OUTER_BOUND('',#812,.T.);
#536=FACE_OUTER_BOUND('',#813,.T.);
#537=FACE_OUTER_BOUND('',#814,.T.);
#538=FACE_OUTER_BOUND('',#815,.T.);
#539=FACE_OUTER_BOUND('',#816,.T.);
#540=FACE_OUTER_BOUND('',#817,.T.);
#541=FACE_OUTER_BOUND('',#818,.T.);
#542=FACE_OUTER_BOUND('',#819,.T.);
#543=FACE_OUTER_BOUND('',#820,.T.);
#544=FACE_OUTER_BOUND('',#821,.T.);
#545=FACE_OUTER_BOUND('',#822,.T.);
#546=FACE_OUTER_BOUND('',#823,.T.);
#547=FACE_OUTER_BOUND('',#824,.T.);
#548=FACE_OUTER_BOUND('',#825,.T.);
#549=FACE_OUTER_BOUND('',#826,.T.);
#550=FACE_OUTER_BOUND('',#827,.T.);
#551=FACE_OUTER_BOUND('',#828,.T.);
#552=FACE_OUTER_BOUND('',#829,.T.);
#553=FACE_OUTER_BOUND('',#830,.T.);
#554=FACE_OUTER_BOUND('',#831,.T.);
#555=FACE_OUTER_BOUND('',#832,.T.);
#556=FACE_OUTER_BOUND('',#833,.T.);
#557=FACE_OUTER_BOUND('',#834,.T.);
#558=FACE_OUTER_BOUND('',#835,.T.);
#559=FACE_OUTER_BOUND('',#836,.T.);
#560=FACE_OUTER_BOUND('',#837,.T.);
#561=FACE_OUTER_BOUND('',#838,.T.);
#562=FACE_OUTER_BOUND('',#839,.T.);
#563=FACE_OUTER_BOUND('',#840,.T.);
#564=FACE_OUTER_BOUND('',#841,.T.);
#565=FACE_OUTER_BOUND('',#842,.T.);
#566=FACE_OUTER_BOUND('',#843,.T.);
#567=FACE_OUTER_BOUND('',#844,.T.);
#568=FACE_OUTER_BOUND('',#845,.T.);
#569=FACE_OUTER_BOUND('',#846,.T.);
#570=FACE_OUTER_BOUND('',#847,.T.);
#571=FACE_OUTER_BOUND('',#848,.T.);
#572=FACE_OUTER_BOUND('',#849,.T.);
#573=FACE_OUTER_BOUND('',#850,.T.);
#574=FACE_OUTER_BOUND('',#851,.T.);
#575=FACE_OUTER_BOUND('',#852,.T.);
#576=FACE_OUTER_BOUND('',#853,.T.);
#577=FACE_OUTER_BOUND('',#854,.T.);
#578=FACE_OUTER_BOUND('',#855,.T.);
#579=FACE_OUTER_BOUND('',#856,.T.);
#580=FACE_OUTER_BOUND('',#857,.T.);
#581=FACE_OUTER_BOUND('',#858,.T.);
#582=FACE_OUTER_BOUND('',#859,.T.);
#583=FACE_OUTER_BOUND('',#860,.T.);
#584=FACE_OUTER_BOUND('',#861,.T.);
#585=FACE_OUTER_BOUND('',#862,.T.);
#586=FACE_OUTER_BOUND('',#863,.T.);
#587=FACE_OUTER_BOUND('',#864,.T.);
#588=FACE_OUTER_BOUND('',#865,.T.);
#589=FACE_OUTER_BOUND('',#866,.T.);
#590=FACE_OUTER_BOUND('',#867,.T.);
#591=FACE_OUTER_BOUND('',#868,.T.);
#592=FACE_OUTER_BOUND('',#869,.T.);
#593=FACE_OUTER_BOUND('',#870,.T.);
#594=FACE_OUTER_BOUND('',#871,.T.);
#595=FACE_OUTER_BOUND('',#872,.T.);
#596=FACE_OUTER_BOUND('',#873,.T.);
#597=FACE_OUTER_BOUND('',#874,.T.);
#598=FACE_OUTER_BOUND('',#875,.T.);
#599=FACE_OUTER_BOUND('',#876,.T.);
#600=FACE_OUTER_BOUND('',#877,.T.);
#601=FACE_OUTER_BOUND('',#878,.T.);
#602=FACE_OUTER_BOUND('',#879,.T.);
#603=FACE_OUTER_BOUND('',#880,.T.);
#604=FACE_OUTER_BOUND('',#881,.T.);
#605=FACE_OUTER_BOUND('',#882,.T.);
#606=FACE_OUTER_BOUND('',#883,.T.);
#607=FACE_OUTER_BOUND('',#884,.T.);
#608=FACE_OUTER_BOUND('',#885,.T.);
#609=FACE_OUTER_BOUND('',#886,.T.);
#610=FACE_OUTER_BOUND('',#887,.T.);
#611=FACE_OUTER_BOUND('',#888,.T.);
#612=FACE_OUTER_BOUND('',#889,.T.);
#613=FACE_OUTER_BOUND('',#890,.T.);
#614=FACE_OUTER_BOUND('',#891,.T.);
#615=FACE_OUTER_BOUND('',#892,.T.);
#616=FACE_OUTER_BOUND('',#893,.T.);
#617=FACE_OUTER_BOUND('',#894,.T.);
#618=FACE_OUTER_BOUND('',#895,.T.);
#619=FACE_OUTER_BOUND('',#896,.T.);
#620=FACE_OUTER_BOUND('',#897,.T.);
#621=FACE_OUTER_BOUND('',#898,.T.);
#622=FACE_OUTER_BOUND('',#899,.T.);
#623=FACE_OUTER_BOUND('',#900,.T.);
#624=FACE_OUTER_BOUND('',#901,.T.);
#625=FACE_OUTER_BOUND('',#902,.T.);
#626=FACE_OUTER_BOUND('',#903,.T.);
#627=FACE_OUTER_BOUND('',#904,.T.);
#628=FACE_OUTER_BOUND('',#905,.T.);
#629=FACE_OUTER_BOUND('',#906,.T.);
#630=FACE_OUTER_BOUND('',#907,.T.);
#631=FACE_OUTER_BOUND('',#908,.T.);
#632=FACE_OUTER_BOUND('',#909,.T.);
#633=FACE_OUTER_BOUND('',#910,.T.);
#634=FACE_OUTER_BOUND('',#911,.T.);
#635=FACE_OUTER_BOUND('',#912,.T.);
#636=FACE_OUTER_BOUND('',#913,.T.);
#637=FACE_OUTER_BOUND('',#914,.T.);
#638=FACE_OUTER_BOUND('',#915,.T.);
#639=FACE_OUTER_BOUND('',#916,.T.);
#640=FACE_OUTER_BOUND('',#917,.T.);
#641=FACE_OUTER_BOUND('',#918,.T.);
#642=FACE_OUTER_BOUND('',#919,.T.);
#643=FACE_OUTER_BOUND('',#920,.T.);
#644=FACE_OUTER_BOUND('',#921,.T.);
#645=FACE_OUTER_BOUND('',#922,.T.);
#646=FACE_OUTER_BOUND('',#923,.T.);
#647=FACE_OUTER_BOUND('',#924,.T.);
#648=FACE_OUTER_BOUND('',#925,.T.);
#649=FACE_OUTER_BOUND('',#926,.T.);
#650=FACE_OUTER_BOUND('',#927,.T.);
#651=FACE_OUTER_BOUND('',#928,.T.);
#652=FACE_OUTER_BOUND('',#929,.T.);
#653=FACE_OUTER_BOUND('',#930,.T.);
#654=FACE_OUTER_BOUND('',#931,.T.);
#655=FACE_OUTER_BOUND('',#932,.T.);
#656=FACE_OUTER_BOUND('',#933,.T.);
#657=FACE_OUTER_BOUND('',#950,.T.);
#658=FACE_OUTER_BOUND('',#967,.T.);
#659=FACE_OUTER_BOUND('',#968,.T.);
#660=FACE_OUTER_BOUND('',#969,.T.);
#661=FACE_OUTER_BOUND('',#970,.T.);
#662=FACE_OUTER_BOUND('',#971,.T.);
#663=FACE_OUTER_BOUND('',#972,.T.);
#664=FACE_OUTER_BOUND('',#974,.T.);
#665=FACE_OUTER_BOUND('',#976,.T.);
#666=FACE_OUTER_BOUND('',#977,.T.);
#667=FACE_OUTER_BOUND('',#978,.T.);
#668=FACE_OUTER_BOUND('',#979,.T.);
#669=FACE_OUTER_BOUND('',#980,.T.);
#670=FACE_OUTER_BOUND('',#981,.T.);
#671=FACE_OUTER_BOUND('',#982,.T.);
#672=FACE_OUTER_BOUND('',#983,.T.);
#673=FACE_OUTER_BOUND('',#984,.T.);
#674=FACE_OUTER_BOUND('',#985,.T.);
#675=FACE_OUTER_BOUND('',#986,.T.);
#676=FACE_OUTER_BOUND('',#988,.T.);
#677=FACE_OUTER_BOUND('',#990,.T.);
#678=FACE_OUTER_BOUND('',#991,.T.);
#679=FACE_OUTER_BOUND('',#992,.T.);
#680=FACE_OUTER_BOUND('',#993,.T.);
#681=FACE_OUTER_BOUND('',#995,.T.);
#682=FACE_OUTER_BOUND('',#996,.T.);
#683=FACE_OUTER_BOUND('',#997,.T.);
#684=FACE_OUTER_BOUND('',#998,.T.);
#685=FACE_OUTER_BOUND('',#999,.T.);
#686=FACE_OUTER_BOUND('',#1000,.T.);
#687=FACE_OUTER_BOUND('',#1001,.T.);
#688=FACE_OUTER_BOUND('',#1002,.T.);
#689=FACE_OUTER_BOUND('',#1003,.T.);
#690=FACE_OUTER_BOUND('',#1004,.T.);
#691=FACE_OUTER_BOUND('',#1005,.T.);
#692=FACE_OUTER_BOUND('',#1006,.T.);
#693=FACE_OUTER_BOUND('',#1007,.T.);
#694=FACE_OUTER_BOUND('',#1008,.T.);
#695=FACE_OUTER_BOUND('',#1009,.T.);
#696=FACE_OUTER_BOUND('',#1010,.T.);
#697=FACE_OUTER_BOUND('',#1011,.T.);
#698=FACE_OUTER_BOUND('',#1012,.T.);
#699=FACE_OUTER_BOUND('',#1013,.T.);
#700=FACE_OUTER_BOUND('',#1014,.T.);
#701=FACE_OUTER_BOUND('',#1016,.T.);
#702=FACE_OUTER_BOUND('',#1018,.T.);
#703=FACE_OUTER_BOUND('',#1020,.T.);
#704=FACE_OUTER_BOUND('',#1022,.T.);
#705=FACE_OUTER_BOUND('',#1023,.T.);
#706=FACE_OUTER_BOUND('',#1024,.T.);
#707=FACE_OUTER_BOUND('',#1025,.T.);
#708=FACE_OUTER_BOUND('',#1026,.T.);
#709=FACE_OUTER_BOUND('',#1027,.T.);
#710=FACE_OUTER_BOUND('',#1028,.T.);
#711=FACE_OUTER_BOUND('',#1029,.T.);
#712=FACE_OUTER_BOUND('',#1030,.T.);
#713=FACE_OUTER_BOUND('',#1031,.T.);
#714=FACE_OUTER_BOUND('',#1032,.T.);
#715=FACE_OUTER_BOUND('',#1034,.T.);
#716=FACE_OUTER_BOUND('',#1036,.T.);
#717=FACE_OUTER_BOUND('',#1038,.T.);
#718=FACE_OUTER_BOUND('',#1040,.T.);
#719=FACE_OUTER_BOUND('',#1041,.T.);
#720=FACE_OUTER_BOUND('',#1042,.T.);
#721=FACE_OUTER_BOUND('',#1043,.T.);
#722=FACE_OUTER_BOUND('',#1044,.T.);
#723=FACE_OUTER_BOUND('',#1045,.T.);
#724=FACE_OUTER_BOUND('',#1046,.T.);
#725=FACE_OUTER_BOUND('',#1047,.T.);
#726=FACE_OUTER_BOUND('',#1048,.T.);
#727=FACE_OUTER_BOUND('',#1049,.T.);
#728=FACE_OUTER_BOUND('',#1050,.T.);
#729=FACE_OUTER_BOUND('',#1051,.T.);
#730=FACE_OUTER_BOUND('',#1052,.T.);
#731=FACE_OUTER_BOUND('',#1054,.T.);
#732=FACE_OUTER_BOUND('',#1056,.T.);
#733=FACE_OUTER_BOUND('',#1058,.T.);
#734=FACE_OUTER_BOUND('',#1060,.T.);
#735=FACE_OUTER_BOUND('',#1062,.T.);
#736=FACE_OUTER_BOUND('',#1063,.T.);
#737=FACE_OUTER_BOUND('',#1064,.T.);
#738=FACE_OUTER_BOUND('',#1065,.T.);
#739=FACE_OUTER_BOUND('',#1066,.T.);
#740=FACE_OUTER_BOUND('',#1067,.T.);
#741=FACE_OUTER_BOUND('',#1068,.T.);
#742=FACE_OUTER_BOUND('',#1069,.T.);
#743=FACE_OUTER_BOUND('',#1070,.T.);
#744=FACE_OUTER_BOUND('',#1071,.T.);
#745=FACE_OUTER_BOUND('',#1072,.T.);
#746=FACE_OUTER_BOUND('',#1073,.T.);
#747=FACE_OUTER_BOUND('',#1074,.T.);
#748=FACE_OUTER_BOUND('',#1076,.T.);
#749=FACE_OUTER_BOUND('',#1078,.T.);
#750=FACE_OUTER_BOUND('',#1080,.T.);
#751=FACE_OUTER_BOUND('',#1082,.T.);
#752=EDGE_LOOP('',(#3240,#3241,#3242,#3243));
#753=EDGE_LOOP('',(#3244,#3245,#3246,#3247));
#754=EDGE_LOOP('',(#3248,#3249,#3250,#3251));
#755=EDGE_LOOP('',(#3252,#3253,#3254,#3255));
#756=EDGE_LOOP('',(#3256,#3257,#3258,#3259));
#757=EDGE_LOOP('',(#3260,#3261,#3262,#3263));
#758=EDGE_LOOP('',(#3264,#3265,#3266,#3267));
#759=EDGE_LOOP('',(#3268,#3269,#3270,#3271));
#760=EDGE_LOOP('',(#3272,#3273,#3274,#3275));
#761=EDGE_LOOP('',(#3276,#3277,#3278,#3279));
#762=EDGE_LOOP('',(#3280,#3281,#3282,#3283));
#763=EDGE_LOOP('',(#3284,#3285,#3286,#3287));
#764=EDGE_LOOP('',(#3288,#3289,#3290,#3291));
#765=EDGE_LOOP('',(#3292,#3293,#3294,#3295));
#766=EDGE_LOOP('',(#3296,#3297,#3298,#3299));
#767=EDGE_LOOP('',(#3300,#3301,#3302,#3303));
#768=EDGE_LOOP('',(#3304,#3305,#3306,#3307));
#769=EDGE_LOOP('',(#3308,#3309,#3310,#3311));
#770=EDGE_LOOP('',(#3312,#3313,#3314,#3315));
#771=EDGE_LOOP('',(#3316,#3317,#3318,#3319));
#772=EDGE_LOOP('',(#3320,#3321,#3322,#3323));
#773=EDGE_LOOP('',(#3324,#3325,#3326,#3327));
#774=EDGE_LOOP('',(#3328,#3329,#3330,#3331));
#775=EDGE_LOOP('',(#3332,#3333,#3334,#3335));
#776=EDGE_LOOP('',(#3336,#3337,#3338,#3339));
#777=EDGE_LOOP('',(#3340,#3341,#3342,#3343));
#778=EDGE_LOOP('',(#3344,#3345,#3346,#3347));
#779=EDGE_LOOP('',(#3348,#3349,#3350,#3351));
#780=EDGE_LOOP('',(#3352,#3353,#3354,#3355));
#781=EDGE_LOOP('',(#3356,#3357,#3358,#3359));
#782=EDGE_LOOP('',(#3360,#3361,#3362,#3363));
#783=EDGE_LOOP('',(#3364,#3365,#3366,#3367));
#784=EDGE_LOOP('',(#3368,#3369,#3370,#3371));
#785=EDGE_LOOP('',(#3372,#3373,#3374,#3375));
#786=EDGE_LOOP('',(#3376,#3377,#3378,#3379));
#787=EDGE_LOOP('',(#3380,#3381,#3382,#3383));
#788=EDGE_LOOP('',(#3384,#3385,#3386,#3387));
#789=EDGE_LOOP('',(#3388,#3389,#3390,#3391));
#790=EDGE_LOOP('',(#3392,#3393,#3394,#3395));
#791=EDGE_LOOP('',(#3396,#3397,#3398,#3399));
#792=EDGE_LOOP('',(#3400,#3401,#3402,#3403));
#793=EDGE_LOOP('',(#3404,#3405,#3406,#3407));
#794=EDGE_LOOP('',(#3408,#3409,#3410,#3411));
#795=EDGE_LOOP('',(#3412,#3413,#3414,#3415));
#796=EDGE_LOOP('',(#3416,#3417,#3418,#3419));
#797=EDGE_LOOP('',(#3420,#3421,#3422,#3423));
#798=EDGE_LOOP('',(#3424,#3425,#3426,#3427));
#799=EDGE_LOOP('',(#3428,#3429,#3430,#3431));
#800=EDGE_LOOP('',(#3432,#3433,#3434,#3435));
#801=EDGE_LOOP('',(#3436,#3437,#3438,#3439));
#802=EDGE_LOOP('',(#3440,#3441,#3442,#3443));
#803=EDGE_LOOP('',(#3444,#3445,#3446,#3447));
#804=EDGE_LOOP('',(#3448,#3449,#3450,#3451));
#805=EDGE_LOOP('',(#3452,#3453,#3454,#3455));
#806=EDGE_LOOP('',(#3456,#3457,#3458,#3459));
#807=EDGE_LOOP('',(#3460,#3461,#3462,#3463));
#808=EDGE_LOOP('',(#3464,#3465,#3466,#3467));
#809=EDGE_LOOP('',(#3468,#3469,#3470,#3471));
#810=EDGE_LOOP('',(#3472,#3473,#3474,#3475));
#811=EDGE_LOOP('',(#3476,#3477,#3478,#3479));
#812=EDGE_LOOP('',(#3480,#3481,#3482,#3483));
#813=EDGE_LOOP('',(#3484,#3485,#3486,#3487));
#814=EDGE_LOOP('',(#3488,#3489,#3490,#3491));
#815=EDGE_LOOP('',(#3492,#3493,#3494,#3495));
#816=EDGE_LOOP('',(#3496,#3497,#3498,#3499));
#817=EDGE_LOOP('',(#3500,#3501,#3502,#3503));
#818=EDGE_LOOP('',(#3504,#3505,#3506,#3507));
#819=EDGE_LOOP('',(#3508,#3509,#3510,#3511));
#820=EDGE_LOOP('',(#3512,#3513,#3514,#3515));
#821=EDGE_LOOP('',(#3516,#3517,#3518,#3519));
#822=EDGE_LOOP('',(#3520,#3521,#3522,#3523));
#823=EDGE_LOOP('',(#3524,#3525,#3526,#3527));
#824=EDGE_LOOP('',(#3528,#3529,#3530,#3531));
#825=EDGE_LOOP('',(#3532,#3533,#3534,#3535));
#826=EDGE_LOOP('',(#3536,#3537,#3538,#3539));
#827=EDGE_LOOP('',(#3540,#3541,#3542,#3543));
#828=EDGE_LOOP('',(#3544,#3545,#3546,#3547));
#829=EDGE_LOOP('',(#3548,#3549,#3550,#3551));
#830=EDGE_LOOP('',(#3552,#3553,#3554,#3555));
#831=EDGE_LOOP('',(#3556,#3557,#3558,#3559));
#832=EDGE_LOOP('',(#3560,#3561,#3562,#3563));
#833=EDGE_LOOP('',(#3564,#3565,#3566,#3567));
#834=EDGE_LOOP('',(#3568,#3569,#3570,#3571));
#835=EDGE_LOOP('',(#3572,#3573,#3574,#3575));
#836=EDGE_LOOP('',(#3576,#3577,#3578,#3579));
#837=EDGE_LOOP('',(#3580,#3581,#3582,#3583));
#838=EDGE_LOOP('',(#3584,#3585,#3586,#3587));
#839=EDGE_LOOP('',(#3588,#3589,#3590,#3591));
#840=EDGE_LOOP('',(#3592,#3593,#3594,#3595));
#841=EDGE_LOOP('',(#3596,#3597,#3598,#3599));
#842=EDGE_LOOP('',(#3600,#3601,#3602,#3603));
#843=EDGE_LOOP('',(#3604,#3605,#3606,#3607));
#844=EDGE_LOOP('',(#3608,#3609,#3610,#3611));
#845=EDGE_LOOP('',(#3612,#3613,#3614,#3615));
#846=EDGE_LOOP('',(#3616,#3617,#3618,#3619));
#847=EDGE_LOOP('',(#3620,#3621,#3622,#3623));
#848=EDGE_LOOP('',(#3624,#3625,#3626,#3627));
#849=EDGE_LOOP('',(#3628,#3629,#3630,#3631));
#850=EDGE_LOOP('',(#3632,#3633,#3634,#3635));
#851=EDGE_LOOP('',(#3636,#3637,#3638,#3639));
#852=EDGE_LOOP('',(#3640,#3641,#3642,#3643));
#853=EDGE_LOOP('',(#3644,#3645,#3646,#3647));
#854=EDGE_LOOP('',(#3648,#3649,#3650,#3651));
#855=EDGE_LOOP('',(#3652,#3653,#3654,#3655));
#856=EDGE_LOOP('',(#3656,#3657,#3658,#3659));
#857=EDGE_LOOP('',(#3660,#3661,#3662,#3663));
#858=EDGE_LOOP('',(#3664,#3665,#3666,#3667));
#859=EDGE_LOOP('',(#3668,#3669,#3670,#3671));
#860=EDGE_LOOP('',(#3672,#3673,#3674,#3675));
#861=EDGE_LOOP('',(#3676,#3677,#3678,#3679));
#862=EDGE_LOOP('',(#3680,#3681,#3682,#3683));
#863=EDGE_LOOP('',(#3684,#3685,#3686,#3687));
#864=EDGE_LOOP('',(#3688,#3689,#3690,#3691));
#865=EDGE_LOOP('',(#3692,#3693,#3694,#3695));
#866=EDGE_LOOP('',(#3696,#3697,#3698,#3699));
#867=EDGE_LOOP('',(#3700,#3701,#3702,#3703));
#868=EDGE_LOOP('',(#3704,#3705,#3706,#3707));
#869=EDGE_LOOP('',(#3708,#3709,#3710,#3711));
#870=EDGE_LOOP('',(#3712,#3713,#3714,#3715));
#871=EDGE_LOOP('',(#3716,#3717,#3718,#3719));
#872=EDGE_LOOP('',(#3720,#3721,#3722,#3723));
#873=EDGE_LOOP('',(#3724,#3725,#3726,#3727));
#874=EDGE_LOOP('',(#3728,#3729,#3730,#3731));
#875=EDGE_LOOP('',(#3732,#3733,#3734,#3735));
#876=EDGE_LOOP('',(#3736,#3737,#3738,#3739));
#877=EDGE_LOOP('',(#3740,#3741,#3742,#3743));
#878=EDGE_LOOP('',(#3744,#3745,#3746,#3747));
#879=EDGE_LOOP('',(#3748,#3749,#3750,#3751));
#880=EDGE_LOOP('',(#3752,#3753,#3754,#3755));
#881=EDGE_LOOP('',(#3756,#3757,#3758,#3759));
#882=EDGE_LOOP('',(#3760,#3761,#3762,#3763));
#883=EDGE_LOOP('',(#3764,#3765,#3766,#3767));
#884=EDGE_LOOP('',(#3768,#3769,#3770,#3771));
#885=EDGE_LOOP('',(#3772,#3773,#3774,#3775));
#886=EDGE_LOOP('',(#3776,#3777,#3778,#3779));
#887=EDGE_LOOP('',(#3780,#3781,#3782,#3783));
#888=EDGE_LOOP('',(#3784,#3785,#3786,#3787));
#889=EDGE_LOOP('',(#3788,#3789,#3790,#3791));
#890=EDGE_LOOP('',(#3792,#3793,#3794,#3795));
#891=EDGE_LOOP('',(#3796,#3797,#3798,#3799));
#892=EDGE_LOOP('',(#3800,#3801,#3802,#3803));
#893=EDGE_LOOP('',(#3804,#3805,#3806,#3807));
#894=EDGE_LOOP('',(#3808,#3809,#3810,#3811));
#895=EDGE_LOOP('',(#3812,#3813,#3814,#3815));
#896=EDGE_LOOP('',(#3816,#3817,#3818,#3819));
#897=EDGE_LOOP('',(#3820,#3821,#3822,#3823));
#898=EDGE_LOOP('',(#3824,#3825,#3826,#3827));
#899=EDGE_LOOP('',(#3828,#3829,#3830,#3831));
#900=EDGE_LOOP('',(#3832,#3833,#3834,#3835));
#901=EDGE_LOOP('',(#3836,#3837,#3838,#3839));
#902=EDGE_LOOP('',(#3840,#3841,#3842,#3843));
#903=EDGE_LOOP('',(#3844,#3845,#3846,#3847));
#904=EDGE_LOOP('',(#3848,#3849,#3850,#3851));
#905=EDGE_LOOP('',(#3852,#3853,#3854,#3855));
#906=EDGE_LOOP('',(#3856,#3857,#3858,#3859));
#907=EDGE_LOOP('',(#3860,#3861,#3862,#3863));
#908=EDGE_LOOP('',(#3864,#3865,#3866,#3867));
#909=EDGE_LOOP('',(#3868,#3869,#3870,#3871));
#910=EDGE_LOOP('',(#3872,#3873,#3874,#3875));
#911=EDGE_LOOP('',(#3876,#3877,#3878,#3879));
#912=EDGE_LOOP('',(#3880,#3881,#3882,#3883));
#913=EDGE_LOOP('',(#3884,#3885,#3886,#3887));
#914=EDGE_LOOP('',(#3888,#3889,#3890,#3891));
#915=EDGE_LOOP('',(#3892,#3893,#3894,#3895));
#916=EDGE_LOOP('',(#3896,#3897,#3898,#3899));
#917=EDGE_LOOP('',(#3900,#3901,#3902,#3903));
#918=EDGE_LOOP('',(#3904,#3905,#3906,#3907));
#919=EDGE_LOOP('',(#3908,#3909,#3910,#3911));
#920=EDGE_LOOP('',(#3912,#3913,#3914,#3915));
#921=EDGE_LOOP('',(#3916,#3917,#3918,#3919));
#922=EDGE_LOOP('',(#3920,#3921,#3922,#3923));
#923=EDGE_LOOP('',(#3924,#3925,#3926,#3927));
#924=EDGE_LOOP('',(#3928,#3929,#3930,#3931));
#925=EDGE_LOOP('',(#3932,#3933,#3934,#3935));
#926=EDGE_LOOP('',(#3936,#3937,#3938,#3939));
#927=EDGE_LOOP('',(#3940,#3941,#3942,#3943));
#928=EDGE_LOOP('',(#3944,#3945,#3946,#3947));
#929=EDGE_LOOP('',(#3948,#3949,#3950,#3951));
#930=EDGE_LOOP('',(#3952,#3953,#3954,#3955));
#931=EDGE_LOOP('',(#3956,#3957,#3958,#3959));
#932=EDGE_LOOP('',(#3960,#3961,#3962,#3963));
#933=EDGE_LOOP('',(#3964,#3965,#3966,#3967,#3968,#3969,#3970,#3971,#3972,
#3973,#3974,#3975,#3976,#3977,#3978,#3979,#3980,#3981,#3982,#3983,#3984,
#3985,#3986,#3987,#3988,#3989,#3990,#3991,#3992,#3993,#3994,#3995,#3996,
#3997,#3998,#3999,#4000,#4001,#4002,#4003,#4004,#4005,#4006,#4007,#4008,
#4009,#4010,#4011,#4012,#4013,#4014,#4015,#4016,#4017,#4018,#4019,#4020,
#4021,#4022,#4023,#4024,#4025,#4026,#4027,#4028,#4029,#4030,#4031,#4032,
#4033,#4034,#4035,#4036,#4037,#4038,#4039,#4040,#4041,#4042,#4043,#4044,
#4045,#4046,#4047,#4048,#4049,#4050,#4051,#4052,#4053,#4054,#4055,#4056,
#4057,#4058,#4059,#4060,#4061,#4062,#4063,#4064,#4065,#4066,#4067,#4068,
#4069,#4070,#4071,#4072,#4073,#4074,#4075,#4076,#4077,#4078,#4079,#4080,
#4081,#4082,#4083));
#934=EDGE_LOOP('',(#4084,#4085,#4086,#4087));
#935=EDGE_LOOP('',(#4088,#4089,#4090,#4091));
#936=EDGE_LOOP('',(#4092,#4093,#4094,#4095));
#937=EDGE_LOOP('',(#4096,#4097,#4098,#4099));
#938=EDGE_LOOP('',(#4100,#4101,#4102,#4103));
#939=EDGE_LOOP('',(#4104,#4105,#4106,#4107));
#940=EDGE_LOOP('',(#4108,#4109,#4110,#4111));
#941=EDGE_LOOP('',(#4112,#4113,#4114,#4115));
#942=EDGE_LOOP('',(#4116,#4117,#4118,#4119));
#943=EDGE_LOOP('',(#4120,#4121,#4122,#4123));
#944=EDGE_LOOP('',(#4124,#4125,#4126,#4127));
#945=EDGE_LOOP('',(#4128,#4129,#4130,#4131));
#946=EDGE_LOOP('',(#4132,#4133,#4134,#4135));
#947=EDGE_LOOP('',(#4136,#4137,#4138,#4139));
#948=EDGE_LOOP('',(#4140));
#949=EDGE_LOOP('',(#4141,#4142,#4143,#4144));
#950=EDGE_LOOP('',(#4145,#4146,#4147,#4148,#4149,#4150,#4151,#4152,#4153,
#4154,#4155,#4156,#4157,#4158,#4159,#4160,#4161,#4162,#4163,#4164,#4165,
#4166,#4167,#4168,#4169,#4170,#4171,#4172,#4173,#4174,#4175,#4176,#4177,
#4178,#4179,#4180,#4181,#4182,#4183,#4184,#4185,#4186,#4187,#4188,#4189,
#4190,#4191,#4192,#4193,#4194,#4195,#4196,#4197,#4198,#4199,#4200,#4201,
#4202,#4203,#4204,#4205,#4206,#4207,#4208,#4209,#4210,#4211,#4212,#4213,
#4214,#4215,#4216,#4217,#4218,#4219,#4220,#4221,#4222,#4223,#4224,#4225,
#4226,#4227,#4228,#4229,#4230,#4231,#4232,#4233,#4234,#4235,#4236,#4237,
#4238,#4239,#4240,#4241,#4242,#4243,#4244,#4245,#4246,#4247,#4248,#4249,
#4250,#4251,#4252,#4253,#4254,#4255,#4256,#4257,#4258,#4259,#4260,#4261,
#4262,#4263,#4264));
#951=EDGE_LOOP('',(#4265,#4266,#4267,#4268));
#952=EDGE_LOOP('',(#4269,#4270,#4271,#4272));
#953=EDGE_LOOP('',(#4273,#4274,#4275,#4276));
#954=EDGE_LOOP('',(#4277,#4278,#4279,#4280));
#955=EDGE_LOOP('',(#4281,#4282,#4283,#4284));
#956=EDGE_LOOP('',(#4285,#4286,#4287,#4288));
#957=EDGE_LOOP('',(#4289,#4290,#4291,#4292));
#958=EDGE_LOOP('',(#4293,#4294,#4295,#4296));
#959=EDGE_LOOP('',(#4297,#4298,#4299,#4300));
#960=EDGE_LOOP('',(#4301,#4302,#4303,#4304));
#961=EDGE_LOOP('',(#4305,#4306,#4307,#4308));
#962=EDGE_LOOP('',(#4309,#4310,#4311,#4312));
#963=EDGE_LOOP('',(#4313,#4314,#4315,#4316));
#964=EDGE_LOOP('',(#4317,#4318,#4319,#4320));
#965=EDGE_LOOP('',(#4321));
#966=EDGE_LOOP('',(#4322,#4323,#4324,#4325));
#967=EDGE_LOOP('',(#4326,#4327,#4328,#4329));
#968=EDGE_LOOP('',(#4330,#4331,#4332,#4333));
#969=EDGE_LOOP('',(#4334,#4335,#4336,#4337));
#970=EDGE_LOOP('',(#4338,#4339,#4340,#4341));
#971=EDGE_LOOP('',(#4342,#4343,#4344,#4345));
#972=EDGE_LOOP('',(#4346,#4347,#4348,#4349));
#973=EDGE_LOOP('',(#4350));
#974=EDGE_LOOP('',(#4351,#4352,#4353,#4354));
#975=EDGE_LOOP('',(#4355));
#976=EDGE_LOOP('',(#4356,#4357,#4358,#4359));
#977=EDGE_LOOP('',(#4360,#4361,#4362,#4363));
#978=EDGE_LOOP('',(#4364,#4365,#4366,#4367));
#979=EDGE_LOOP('',(#4368,#4369,#4370,#4371));
#980=EDGE_LOOP('',(#4372,#4373,#4374,#4375));
#981=EDGE_LOOP('',(#4376,#4377,#4378,#4379));
#982=EDGE_LOOP('',(#4380,#4381,#4382,#4383));
#983=EDGE_LOOP('',(#4384,#4385,#4386,#4387));
#984=EDGE_LOOP('',(#4388,#4389,#4390,#4391));
#985=EDGE_LOOP('',(#4392,#4393,#4394,#4395));
#986=EDGE_LOOP('',(#4396,#4397,#4398,#4399,#4400,#4401,#4402,#4403,#4404));
#987=EDGE_LOOP('',(#4405));
#988=EDGE_LOOP('',(#4406,#4407,#4408,#4409,#4410,#4411,#4412,#4413,#4414));
#989=EDGE_LOOP('',(#4415));
#990=EDGE_LOOP('',(#4416,#4417,#4418,#4419));
#991=EDGE_LOOP('',(#4420));
#992=EDGE_LOOP('',(#4421));
#993=EDGE_LOOP('',(#4422));
#994=EDGE_LOOP('',(#4423));
#995=EDGE_LOOP('',(#4424,#4425,#4426,#4427));
#996=EDGE_LOOP('',(#4428,#4429,#4430,#4431,#4432));
#997=EDGE_LOOP('',(#4433,#4434,#4435,#4436));
#998=EDGE_LOOP('',(#4437,#4438));
#999=EDGE_LOOP('',(#4439,#4440,#4441,#4442,#4443,#4444,#4445,#4446,#4447,
#4448,#4449,#4450));
#1000=EDGE_LOOP('',(#4451,#4452));
#1001=EDGE_LOOP('',(#4453));
#1002=EDGE_LOOP('',(#4454,#4455,#4456,#4457));
#1003=EDGE_LOOP('',(#4458,#4459,#4460,#4461));
#1004=EDGE_LOOP('',(#4462));
#1005=EDGE_LOOP('',(#4463));
#1006=EDGE_LOOP('',(#4464,#4465,#4466,#4467));
#1007=EDGE_LOOP('',(#4468,#4469,#4470,#4471));
#1008=EDGE_LOOP('',(#4472,#4473,#4474,#4475,#4476));
#1009=EDGE_LOOP('',(#4477,#4478,#4479,#4480,#4481));
#1010=EDGE_LOOP('',(#4482,#4483,#4484,#4485));
#1011=EDGE_LOOP('',(#4486,#4487,#4488,#4489));
#1012=EDGE_LOOP('',(#4490,#4491,#4492,#4493));
#1013=EDGE_LOOP('',(#4494,#4495,#4496,#4497));
#1014=EDGE_LOOP('',(#4498));
#1015=EDGE_LOOP('',(#4499));
#1016=EDGE_LOOP('',(#4500));
#1017=EDGE_LOOP('',(#4501));
#1018=EDGE_LOOP('',(#4502));
#1019=EDGE_LOOP('',(#4503));
#1020=EDGE_LOOP('',(#4504));
#1021=EDGE_LOOP('',(#4505));
#1022=EDGE_LOOP('',(#4506,#4507,#4508,#4509,#4510));
#1023=EDGE_LOOP('',(#4511,#4512,#4513,#4514,#4515));
#1024=EDGE_LOOP('',(#4516,#4517,#4518,#4519));
#1025=EDGE_LOOP('',(#4520,#4521,#4522,#4523));
#1026=EDGE_LOOP('',(#4524,#4525,#4526,#4527));
#1027=EDGE_LOOP('',(#4528,#4529,#4530,#4531));
#1028=EDGE_LOOP('',(#4532,#4533,#4534,#4535));
#1029=EDGE_LOOP('',(#4536,#4537,#4538,#4539));
#1030=EDGE_LOOP('',(#4540,#4541,#4542,#4543));
#1031=EDGE_LOOP('',(#4544,#4545,#4546,#4547));
#1032=EDGE_LOOP('',(#4548));
#1033=EDGE_LOOP('',(#4549));
#1034=EDGE_LOOP('',(#4550));
#1035=EDGE_LOOP('',(#4551));
#1036=EDGE_LOOP('',(#4552));
#1037=EDGE_LOOP('',(#4553));
#1038=EDGE_LOOP('',(#4554));
#1039=EDGE_LOOP('',(#4555));
#1040=EDGE_LOOP('',(#4556,#4557,#4558,#4559));
#1041=EDGE_LOOP('',(#4560,#4561,#4562,#4563));
#1042=EDGE_LOOP('',(#4564,#4565,#4566,#4567));
#1043=EDGE_LOOP('',(#4568,#4569,#4570,#4571));
#1044=EDGE_LOOP('',(#4572,#4573,#4574,#4575));
#1045=EDGE_LOOP('',(#4576,#4577,#4578,#4579));
#1046=EDGE_LOOP('',(#4580,#4581,#4582,#4583));
#1047=EDGE_LOOP('',(#4584,#4585,#4586,#4587));
#1048=EDGE_LOOP('',(#4588,#4589,#4590,#4591));
#1049=EDGE_LOOP('',(#4592,#4593,#4594,#4595));
#1050=EDGE_LOOP('',(#4596,#4597,#4598,#4599));
#1051=EDGE_LOOP('',(#4600,#4601,#4602,#4603));
#1052=EDGE_LOOP('',(#4604));
#1053=EDGE_LOOP('',(#4605));
#1054=EDGE_LOOP('',(#4606));
#1055=EDGE_LOOP('',(#4607));
#1056=EDGE_LOOP('',(#4608));
#1057=EDGE_LOOP('',(#4609));
#1058=EDGE_LOOP('',(#4610));
#1059=EDGE_LOOP('',(#4611));
#1060=EDGE_LOOP('',(#4612));
#1061=EDGE_LOOP('',(#4613));
#1062=EDGE_LOOP('',(#4614,#4615,#4616,#4617));
#1063=EDGE_LOOP('',(#4618,#4619,#4620,#4621));
#1064=EDGE_LOOP('',(#4622,#4623,#4624,#4625));
#1065=EDGE_LOOP('',(#4626,#4627,#4628,#4629));
#1066=EDGE_LOOP('',(#4630,#4631,#4632,#4633));
#1067=EDGE_LOOP('',(#4634,#4635,#4636,#4637));
#1068=EDGE_LOOP('',(#4638,#4639,#4640,#4641));
#1069=EDGE_LOOP('',(#4642,#4643,#4644,#4645));
#1070=EDGE_LOOP('',(#4646,#4647,#4648,#4649));
#1071=EDGE_LOOP('',(#4650,#4651,#4652,#4653));
#1072=EDGE_LOOP('',(#4654,#4655,#4656,#4657));
#1073=EDGE_LOOP('',(#4658,#4659,#4660,#4661));
#1074=EDGE_LOOP('',(#4662));
#1075=EDGE_LOOP('',(#4663));
#1076=EDGE_LOOP('',(#4664));
#1077=EDGE_LOOP('',(#4665));
#1078=EDGE_LOOP('',(#4666));
#1079=EDGE_LOOP('',(#4667));
#1080=EDGE_LOOP('',(#4668));
#1081=EDGE_LOOP('',(#4669));
#1082=EDGE_LOOP('',(#4670));
#1083=EDGE_LOOP('',(#4671));
#1084=LINE('',#7252,#1569);
#1085=LINE('',#7254,#1570);
#1086=LINE('',#7256,#1571);
#1087=LINE('',#7257,#1572);
#1088=LINE('',#7260,#1573);
#1089=LINE('',#7262,#1574);
#1090=LINE('',#7263,#1575);
#1091=LINE('',#7266,#1576);
#1092=LINE('',#7268,#1577);
#1093=LINE('',#7269,#1578);
#1094=LINE('',#7274,#1579);
#1095=LINE('',#7280,#1580);
#1096=LINE('',#7285,#1581);
#1097=LINE('',#7287,#1582);
#1098=LINE('',#7289,#1583);
#1099=LINE('',#7290,#1584);
#1100=LINE('',#7293,#1585);
#1101=LINE('',#7295,#1586);
#1102=LINE('',#7296,#1587);
#1103=LINE('',#7299,#1588);
#1104=LINE('',#7301,#1589);
#1105=LINE('',#7302,#1590);
#1106=LINE('',#7307,#1591);
#1107=LINE('',#7313,#1592);
#1108=LINE('',#7317,#1593);
#1109=LINE('',#7319,#1594);
#1110=LINE('',#7320,#1595);
#1111=LINE('',#7323,#1596);
#1112=LINE('',#7325,#1597);
#1113=LINE('',#7326,#1598);
#1114=LINE('',#7329,#1599);
#1115=LINE('',#7331,#1600);
#1116=LINE('',#7332,#1601);
#1117=LINE('',#7337,#1602);
#1118=LINE('',#7342,#1603);
#1119=LINE('',#7344,#1604);
#1120=LINE('',#7346,#1605);
#1121=LINE('',#7347,#1606);
#1122=LINE('',#7350,#1607);
#1123=LINE('',#7352,#1608);
#1124=LINE('',#7353,#1609);
#1125=LINE('',#7356,#1610);
#1126=LINE('',#7358,#1611);
#1127=LINE('',#7359,#1612);
#1128=LINE('',#7364,#1613);
#1129=LINE('',#7370,#1614);
#1130=LINE('',#7374,#1615);
#1131=LINE('',#7376,#1616);
#1132=LINE('',#7377,#1617);
#1133=LINE('',#7380,#1618);
#1134=LINE('',#7382,#1619);
#1135=LINE('',#7383,#1620);
#1136=LINE('',#7385,#1621);
#1137=LINE('',#7386,#1622);
#1138=LINE('',#7389,#1623);
#1139=LINE('',#7391,#1624);
#1140=LINE('',#7392,#1625);
#1141=LINE('',#7395,#1626);
#1142=LINE('',#7397,#1627);
#1143=LINE('',#7398,#1628);
#1144=LINE('',#7401,#1629);
#1145=LINE('',#7403,#1630);
#1146=LINE('',#7404,#1631);
#1147=LINE('',#7409,#1632);
#1148=LINE('',#7414,#1633);
#1149=LINE('',#7416,#1634);
#1150=LINE('',#7418,#1635);
#1151=LINE('',#7419,#1636);
#1152=LINE('',#7422,#1637);
#1153=LINE('',#7424,#1638);
#1154=LINE('',#7425,#1639);
#1155=LINE('',#7427,#1640);
#1156=LINE('',#7428,#1641);
#1157=LINE('',#7433,#1642);
#1158=LINE('',#7437,#1643);
#1159=LINE('',#7439,#1644);
#1160=LINE('',#7440,#1645);
#1161=LINE('',#7443,#1646);
#1162=LINE('',#7445,#1647);
#1163=LINE('',#7446,#1648);
#1164=LINE('',#7448,#1649);
#1165=LINE('',#7449,#1650);
#1166=LINE('',#7453,#1651);
#1167=LINE('',#7455,#1652);
#1168=LINE('',#7457,#1653);
#1169=LINE('',#7458,#1654);
#1170=LINE('',#7462,#1655);
#1171=LINE('',#7464,#1656);
#1172=LINE('',#7466,#1657);
#1173=LINE('',#7467,#1658);
#1174=LINE('',#7472,#1659);
#1175=LINE('',#7478,#1660);
#1176=LINE('',#7484,#1661);
#1177=LINE('',#7490,#1662);
#1178=LINE('',#7493,#1663);
#1179=LINE('',#7494,#1664);
#1180=LINE('',#7498,#1665);
#1181=LINE('',#7500,#1666);
#1182=LINE('',#7502,#1667);
#1183=LINE('',#7503,#1668);
#1184=LINE('',#7508,#1669);
#1185=LINE('',#7514,#1670);
#1186=LINE('',#7519,#1671);
#1187=LINE('',#7521,#1672);
#1188=LINE('',#7523,#1673);
#1189=LINE('',#7524,#1674);
#1190=LINE('',#7526,#1675);
#1191=LINE('',#7527,#1676);
#1192=LINE('',#7532,#1677);
#1193=LINE('',#7538,#1678);
#1194=LINE('',#7543,#1679);
#1195=LINE('',#7545,#1680);
#1196=LINE('',#7547,#1681);
#1197=LINE('',#7548,#1682);
#1198=LINE('',#7551,#1683);
#1199=LINE('',#7553,#1684);
#1200=LINE('',#7554,#1685);
#1201=LINE('',#7557,#1686);
#1202=LINE('',#7559,#1687);
#1203=LINE('',#7560,#1688);
#1204=LINE('',#7565,#1689);
#1205=LINE('',#7571,#1690);
#1206=LINE('',#7576,#1691);
#1207=LINE('',#7578,#1692);
#1208=LINE('',#7580,#1693);
#1209=LINE('',#7581,#1694);
#1210=LINE('',#7584,#1695);
#1211=LINE('',#7586,#1696);
#1212=LINE('',#7587,#1697);
#1213=LINE('',#7590,#1698);
#1214=LINE('',#7592,#1699);
#1215=LINE('',#7593,#1700);
#1216=LINE('',#7598,#1701);
#1217=LINE('',#7604,#1702);
#1218=LINE('',#7608,#1703);
#1219=LINE('',#7610,#1704);
#1220=LINE('',#7611,#1705);
#1221=LINE('',#7614,#1706);
#1222=LINE('',#7616,#1707);
#1223=LINE('',#7617,#1708);
#1224=LINE('',#7620,#1709);
#1225=LINE('',#7622,#1710);
#1226=LINE('',#7623,#1711);
#1227=LINE('',#7628,#1712);
#1228=LINE('',#7632,#1713);
#1229=LINE('',#7634,#1714);
#1230=LINE('',#7635,#1715);
#1231=LINE('',#7638,#1716);
#1232=LINE('',#7640,#1717);
#1233=LINE('',#7641,#1718);
#1234=LINE('',#7643,#1719);
#1235=LINE('',#7644,#1720);
#1236=LINE('',#7647,#1721);
#1237=LINE('',#7649,#1722);
#1238=LINE('',#7650,#1723);
#1239=LINE('',#7653,#1724);
#1240=LINE('',#7655,#1725);
#1241=LINE('',#7656,#1726);
#1242=LINE('',#7659,#1727);
#1243=LINE('',#7661,#1728);
#1244=LINE('',#7662,#1729);
#1245=LINE('',#7667,#1730);
#1246=LINE('',#7671,#1731);
#1247=LINE('',#7673,#1732);
#1248=LINE('',#7674,#1733);
#1249=LINE('',#7677,#1734);
#1250=LINE('',#7679,#1735);
#1251=LINE('',#7680,#1736);
#1252=LINE('',#7682,#1737);
#1253=LINE('',#7683,#1738);
#1254=LINE('',#7687,#1739);
#1255=LINE('',#7689,#1740);
#1256=LINE('',#7691,#1741);
#1257=LINE('',#7692,#1742);
#1258=LINE('',#7696,#1743);
#1259=LINE('',#7698,#1744);
#1260=LINE('',#7700,#1745);
#1261=LINE('',#7701,#1746);
#1262=LINE('',#7706,#1747);
#1263=LINE('',#7712,#1748);
#1264=LINE('',#7718,#1749);
#1265=LINE('',#7724,#1750);
#1266=LINE('',#7727,#1751);
#1267=LINE('',#7728,#1752);
#1268=LINE('',#7732,#1753);
#1269=LINE('',#7734,#1754);
#1270=LINE('',#7736,#1755);
#1271=LINE('',#7737,#1756);
#1272=LINE('',#7742,#1757);
#1273=LINE('',#7748,#1758);
#1274=LINE('',#7753,#1759);
#1275=LINE('',#7755,#1760);
#1276=LINE('',#7757,#1761);
#1277=LINE('',#7758,#1762);
#1278=LINE('',#7762,#1763);
#1279=LINE('',#7764,#1764);
#1280=LINE('',#7766,#1765);
#1281=LINE('',#7767,#1766);
#1282=LINE('',#7772,#1767);
#1283=LINE('',#7778,#1768);
#1284=LINE('',#7784,#1769);
#1285=LINE('',#7790,#1770);
#1286=LINE('',#7795,#1771);
#1287=LINE('',#7797,#1772);
#1288=LINE('',#7799,#1773);
#1289=LINE('',#7800,#1774);
#1290=LINE('',#7804,#1775);
#1291=LINE('',#7806,#1776);
#1292=LINE('',#7808,#1777);
#1293=LINE('',#7809,#1778);
#1294=LINE('',#7814,#1779);
#1295=LINE('',#7820,#1780);
#1296=LINE('',#7826,#1781);
#1297=LINE('',#7832,#1782);
#1298=LINE('',#7835,#1783);
#1299=LINE('',#7836,#1784);
#1300=LINE('',#7840,#1785);
#1301=LINE('',#7842,#1786);
#1302=LINE('',#7844,#1787);
#1303=LINE('',#7845,#1788);
#1304=LINE('',#7850,#1789);
#1305=LINE('',#7856,#1790);
#1306=LINE('',#7859,#1791);
#1307=LINE('',#7860,#1792);
#1308=LINE('',#7862,#1793);
#1309=LINE('',#7863,#1794);
#1310=LINE('',#7865,#1795);
#1311=LINE('',#7866,#1796);
#1312=LINE('',#7870,#1797);
#1313=LINE('',#7872,#1798);
#1314=LINE('',#7874,#1799);
#1315=LINE('',#7875,#1800);
#1316=LINE('',#7880,#1801);
#1317=LINE('',#7886,#1802);
#1318=LINE('',#7889,#1803);
#1319=LINE('',#7890,#1804);
#1320=LINE('',#7892,#1805);
#1321=LINE('',#7893,#1806);
#1322=LINE('',#7897,#1807);
#1323=LINE('',#7899,#1808);
#1324=LINE('',#7901,#1809);
#1325=LINE('',#7902,#1810);
#1326=LINE('',#7905,#1811);
#1327=LINE('',#7907,#1812);
#1328=LINE('',#7908,#1813);
#1329=LINE('',#7911,#1814);
#1330=LINE('',#7913,#1815);
#1331=LINE('',#7914,#1816);
#1332=LINE('',#7919,#1817);
#1333=LINE('',#7925,#1818);
#1334=LINE('',#7929,#1819);
#1335=LINE('',#7931,#1820);
#1336=LINE('',#7932,#1821);
#1337=LINE('',#7935,#1822);
#1338=LINE('',#7937,#1823);
#1339=LINE('',#7938,#1824);
#1340=LINE('',#7941,#1825);
#1341=LINE('',#7943,#1826);
#1342=LINE('',#7944,#1827);
#1343=LINE('',#7949,#1828);
#1344=LINE('',#7954,#1829);
#1345=LINE('',#7956,#1830);
#1346=LINE('',#7958,#1831);
#1347=LINE('',#7959,#1832);
#1348=LINE('',#7962,#1833);
#1349=LINE('',#7964,#1834);
#1350=LINE('',#7965,#1835);
#1351=LINE('',#7968,#1836);
#1352=LINE('',#7970,#1837);
#1353=LINE('',#7971,#1838);
#1354=LINE('',#7976,#1839);
#1355=LINE('',#7982,#1840);
#1356=LINE('',#7987,#1841);
#1357=LINE('',#7989,#1842);
#1358=LINE('',#7991,#1843);
#1359=LINE('',#7992,#1844);
#1360=LINE('',#7995,#1845);
#1361=LINE('',#7997,#1846);
#1362=LINE('',#7998,#1847);
#1363=LINE('',#8001,#1848);
#1364=LINE('',#8003,#1849);
#1365=LINE('',#8004,#1850);
#1366=LINE('',#8009,#1851);
#1367=LINE('',#8015,#1852);
#1368=LINE('',#8019,#1853);
#1369=LINE('',#8021,#1854);
#1370=LINE('',#8022,#1855);
#1371=LINE('',#8025,#1856);
#1372=LINE('',#8027,#1857);
#1373=LINE('',#8028,#1858);
#1374=LINE('',#8030,#1859);
#1375=LINE('',#8031,#1860);
#1376=LINE('',#8034,#1861);
#1377=LINE('',#8036,#1862);
#1378=LINE('',#8037,#1863);
#1379=LINE('',#8040,#1864);
#1380=LINE('',#8042,#1865);
#1381=LINE('',#8043,#1866);
#1382=LINE('',#8045,#1867);
#1383=LINE('',#8046,#1868);
#1384=LINE('',#8049,#1869);
#1385=LINE('',#8051,#1870);
#1386=LINE('',#8052,#1871);
#1387=LINE('',#8055,#1872);
#1388=LINE('',#8057,#1873);
#1389=LINE('',#8058,#1874);
#1390=LINE('',#8060,#1875);
#1391=LINE('',#8061,#1876);
#1392=LINE('',#8064,#1877);
#1393=LINE('',#8066,#1878);
#1394=LINE('',#8067,#1879);
#1395=LINE('',#8070,#1880);
#1396=LINE('',#8072,#1881);
#1397=LINE('',#8073,#1882);
#1398=LINE('',#8076,#1883);
#1399=LINE('',#8078,#1884);
#1400=LINE('',#8079,#1885);
#1401=LINE('',#8084,#1886);
#1402=LINE('',#8087,#1887);
#1403=LINE('',#8088,#1888);
#1404=LINE('',#8092,#1889);
#1405=LINE('',#8094,#1890);
#1406=LINE('',#8096,#1891);
#1407=LINE('',#8097,#1892);
#1408=LINE('',#8102,#1893);
#1409=LINE('',#8108,#1894);
#1410=LINE('',#8113,#1895);
#1411=LINE('',#8115,#1896);
#1412=LINE('',#8117,#1897);
#1413=LINE('',#8118,#1898);
#1414=LINE('',#8120,#1899);
#1415=LINE('',#8121,#1900);
#1416=LINE('',#8126,#1901);
#1417=LINE('',#8132,#1902);
#1418=LINE('',#8135,#1903);
#1419=LINE('',#8136,#1904);
#1420=LINE('',#8138,#1905);
#1421=LINE('',#8139,#1906);
#1422=LINE('',#8143,#1907);
#1423=LINE('',#8145,#1908);
#1424=LINE('',#8147,#1909);
#1425=LINE('',#8148,#1910);
#1426=LINE('',#8151,#1911);
#1427=LINE('',#8153,#1912);
#1428=LINE('',#8154,#1913);
#1429=LINE('',#8157,#1914);
#1430=LINE('',#8159,#1915);
#1431=LINE('',#8160,#1916);
#1432=LINE('',#8165,#1917);
#1433=LINE('',#8171,#1918);
#1434=LINE('',#8175,#1919);
#1435=LINE('',#8177,#1920);
#1436=LINE('',#8178,#1921);
#1437=LINE('',#8181,#1922);
#1438=LINE('',#8183,#1923);
#1439=LINE('',#8184,#1924);
#1440=LINE('',#8187,#1925);
#1441=LINE('',#8189,#1926);
#1442=LINE('',#8190,#1927);
#1443=LINE('',#8195,#1928);
#1444=LINE('',#8200,#1929);
#1445=LINE('',#8202,#1930);
#1446=LINE('',#8204,#1931);
#1447=LINE('',#8205,#1932);
#1448=LINE('',#8208,#1933);
#1449=LINE('',#8210,#1934);
#1450=LINE('',#8211,#1935);
#1451=LINE('',#8214,#1936);
#1452=LINE('',#8216,#1937);
#1453=LINE('',#8217,#1938);
#1454=LINE('',#8222,#1939);
#1455=LINE('',#8228,#1940);
#1456=LINE('',#8232,#1941);
#1457=LINE('',#8234,#1942);
#1458=LINE('',#8235,#1943);
#1459=LINE('',#8238,#1944);
#1460=LINE('',#8240,#1945);
#1461=LINE('',#8241,#1946);
#1462=LINE('',#8244,#1947);
#1463=LINE('',#8246,#1948);
#1464=LINE('',#8247,#1949);
#1465=LINE('',#8252,#1950);
#1466=LINE('',#8256,#1951);
#1467=LINE('',#8258,#1952);
#1468=LINE('',#8259,#1953);
#1469=LINE('',#8262,#1954);
#1470=LINE('',#8264,#1955);
#1471=LINE('',#8265,#1956);
#1472=LINE('',#8268,#1957);
#1473=LINE('',#8270,#1958);
#1474=LINE('',#8271,#1959);
#1475=LINE('',#8276,#1960);
#1476=LINE('',#8280,#1961);
#1477=LINE('',#8282,#1962);
#1478=LINE('',#8283,#1963);
#1479=LINE('',#8286,#1964);
#1480=LINE('',#8288,#1965);
#1481=LINE('',#8289,#1966);
#1482=LINE('',#8291,#1967);
#1483=LINE('',#8292,#1968);
#1484=LINE('',#8295,#1969);
#1485=LINE('',#8297,#1970);
#1486=LINE('',#8298,#1971);
#1487=LINE('',#8301,#1972);
#1488=LINE('',#8303,#1973);
#1489=LINE('',#8304,#1974);
#1490=LINE('',#8306,#1975);
#1491=LINE('',#8307,#1976);
#1492=LINE('',#8310,#1977);
#1493=LINE('',#8312,#1978);
#1494=LINE('',#8313,#1979);
#1495=LINE('',#8316,#1980);
#1496=LINE('',#8318,#1981);
#1497=LINE('',#8319,#1982);
#1498=LINE('',#8321,#1983);
#1499=LINE('',#8322,#1984);
#1500=LINE('',#8324,#1985);
#1501=LINE('',#8325,#1986);
#1502=LINE('',#8327,#1987);
#1503=LINE('',#8328,#1988);
#1504=LINE('',#8333,#1989);
#1505=LINE('',#8342,#1990);
#1506=LINE('',#8347,#1991);
#1507=LINE('',#8349,#1992);
#1508=LINE('',#8351,#1993);
#1509=LINE('',#8352,#1994);
#1510=LINE('',#8355,#1995);
#1511=LINE('',#8357,#1996);
#1512=LINE('',#8358,#1997);
#1513=LINE('',#8361,#1998);
#1514=LINE('',#8363,#1999);
#1515=LINE('',#8364,#2000);
#1516=LINE('',#8366,#2001);
#1517=LINE('',#8367,#2002);
#1518=LINE('',#8374,#2003);
#1519=LINE('',#8376,#2004);
#1520=LINE('',#8378,#2005);
#1521=LINE('',#8379,#2006);
#1522=LINE('',#8383,#2007);
#1523=LINE('',#8385,#2008);
#1524=LINE('',#8387,#2009);
#1525=LINE('',#8388,#2010);
#1526=LINE('',#8395,#2011);
#1527=LINE('',#8397,#2012);
#1528=LINE('',#8399,#2013);
#1529=LINE('',#8400,#2014);
#1530=LINE('',#8403,#2015);
#1531=LINE('',#8405,#2016);
#1532=LINE('',#8406,#2017);
#1533=LINE('',#8411,#2018);
#1534=LINE('',#8415,#2019);
#1535=LINE('',#8417,#2020);
#1536=LINE('',#8418,#2021);
#1537=LINE('',#8424,#2022);
#1538=LINE('',#8426,#2023);
#1539=LINE('',#8427,#2024);
#1540=LINE('',#8438,#2025);
#1541=LINE('',#8462,#2026);
#1542=LINE('',#8474,#2027);
#1543=LINE('',#8480,#2028);
#1544=LINE('',#8496,#2029);
#1545=LINE('',#8517,#2030);
#1546=LINE('',#8523,#2031);
#1547=LINE('',#8532,#2032);
#1548=LINE('',#8538,#2033);
#1549=LINE('',#8546,#2034);
#1550=LINE('',#8550,#2035);
#1551=LINE('',#8561,#2036);
#1552=LINE('',#8568,#2037);
#1553=LINE('',#8579,#2038);
#1554=LINE('',#8584,#2039);
#1555=LINE('',#8594,#2040);
#1556=LINE('',#8604,#2041);
#1557=LINE('',#8608,#2042);
#1558=LINE('',#8618,#2043);
#1559=LINE('',#8632,#2044);
#1560=LINE('',#8643,#2045);
#1561=LINE('',#8657,#2046);
#1562=LINE('',#8671,#2047);
#1563=LINE('',#8685,#2048);
#1564=LINE('',#8695,#2049);
#1565=LINE('',#8706,#2050);
#1566=LINE('',#8720,#2051);
#1567=LINE('',#8734,#2052);
#1568=LINE('',#8748,#2053);
#1569=VECTOR('',#5728,10.);
#1570=VECTOR('',#5729,10.);
#1571=VECTOR('',#5730,10.);
#1572=VECTOR('',#5731,10.);
#1573=VECTOR('',#5734,10.);
#1574=VECTOR('',#5735,10.);
#1575=VECTOR('',#5736,10.);
#1576=VECTOR('',#5739,10.);
#1577=VECTOR('',#5740,10.);
#1578=VECTOR('',#5741,10.);
#1579=VECTOR('',#5746,10.);
#1580=VECTOR('',#5753,10.);
#1581=VECTOR('',#5758,10.);
#1582=VECTOR('',#5759,10.);
#1583=VECTOR('',#5760,10.);
#1584=VECTOR('',#5761,10.);
#1585=VECTOR('',#5764,10.);
#1586=VECTOR('',#5765,10.);
#1587=VECTOR('',#5766,10.);
#1588=VECTOR('',#5769,10.);
#1589=VECTOR('',#5770,10.);
#1590=VECTOR('',#5771,10.);
#1591=VECTOR('',#5776,10.);
#1592=VECTOR('',#5783,10.);
#1593=VECTOR('',#5788,10.);
#1594=VECTOR('',#5789,10.);
#1595=VECTOR('',#5790,10.);
#1596=VECTOR('',#5793,10.);
#1597=VECTOR('',#5794,10.);
#1598=VECTOR('',#5795,10.);
#1599=VECTOR('',#5798,10.);
#1600=VECTOR('',#5799,10.);
#1601=VECTOR('',#5800,10.);
#1602=VECTOR('',#5805,10.);
#1603=VECTOR('',#5810,10.);
#1604=VECTOR('',#5811,10.);
#1605=VECTOR('',#5812,10.);
#1606=VECTOR('',#5813,10.);
#1607=VECTOR('',#5816,10.);
#1608=VECTOR('',#5817,10.);
#1609=VECTOR('',#5818,10.);
#1610=VECTOR('',#5821,10.);
#1611=VECTOR('',#5822,10.);
#1612=VECTOR('',#5823,10.);
#1613=VECTOR('',#5828,10.);
#1614=VECTOR('',#5835,10.);
#1615=VECTOR('',#5840,10.);
#1616=VECTOR('',#5841,10.);
#1617=VECTOR('',#5842,10.);
#1618=VECTOR('',#5845,10.);
#1619=VECTOR('',#5846,10.);
#1620=VECTOR('',#5847,10.);
#1621=VECTOR('',#5850,10.);
#1622=VECTOR('',#5851,10.);
#1623=VECTOR('',#5854,10.);
#1624=VECTOR('',#5855,10.);
#1625=VECTOR('',#5856,10.);
#1626=VECTOR('',#5859,10.);
#1627=VECTOR('',#5860,10.);
#1628=VECTOR('',#5861,10.);
#1629=VECTOR('',#5864,10.);
#1630=VECTOR('',#5865,10.);
#1631=VECTOR('',#5866,10.);
#1632=VECTOR('',#5871,10.);
#1633=VECTOR('',#5876,10.);
#1634=VECTOR('',#5877,10.);
#1635=VECTOR('',#5878,10.);
#1636=VECTOR('',#5879,10.);
#1637=VECTOR('',#5882,9.99999999999999);
#1638=VECTOR('',#5883,10.);
#1639=VECTOR('',#5884,10.);
#1640=VECTOR('',#5887,10.);
#1641=VECTOR('',#5888,10.);
#1642=VECTOR('',#5893,10.);
#1643=VECTOR('',#5898,10.);
#1644=VECTOR('',#5899,9.99999999999998);
#1645=VECTOR('',#5900,10.);
#1646=VECTOR('',#5903,10.);
#1647=VECTOR('',#5904,10.);
#1648=VECTOR('',#5905,10.);
#1649=VECTOR('',#5908,10.);
#1650=VECTOR('',#5909,10.);
#1651=VECTOR('',#5912,10.);
#1652=VECTOR('',#5913,10.);
#1653=VECTOR('',#5914,10.);
#1654=VECTOR('',#5915,10.);
#1655=VECTOR('',#5918,10.);
#1656=VECTOR('',#5919,10.);
#1657=VECTOR('',#5920,10.);
#1658=VECTOR('',#5921,10.);
#1659=VECTOR('',#5926,10.);
#1660=VECTOR('',#5933,10.);
#1661=VECTOR('',#5940,10.);
#1662=VECTOR('',#5947,10.);
#1663=VECTOR('',#5952,10.);
#1664=VECTOR('',#5953,10.);
#1665=VECTOR('',#5956,10.);
#1666=VECTOR('',#5957,10.);
#1667=VECTOR('',#5958,10.);
#1668=VECTOR('',#5959,10.);
#1669=VECTOR('',#5964,10.);
#1670=VECTOR('',#5971,10.);
#1671=VECTOR('',#5976,10.);
#1672=VECTOR('',#5977,10.);
#1673=VECTOR('',#5978,10.);
#1674=VECTOR('',#5979,10.);
#1675=VECTOR('',#5982,10.);
#1676=VECTOR('',#5983,10.);
#1677=VECTOR('',#5988,10.);
#1678=VECTOR('',#5995,10.);
#1679=VECTOR('',#6000,10.);
#1680=VECTOR('',#6001,10.);
#1681=VECTOR('',#6002,10.);
#1682=VECTOR('',#6003,10.);
#1683=VECTOR('',#6006,10.);
#1684=VECTOR('',#6007,9.99999999999999);
#1685=VECTOR('',#6008,10.);
#1686=VECTOR('',#6011,10.);
#1687=VECTOR('',#6012,10.);
#1688=VECTOR('',#6013,10.);
#1689=VECTOR('',#6018,10.);
#1690=VECTOR('',#6025,10.);
#1691=VECTOR('',#6030,9.99999999999998);
#1692=VECTOR('',#6031,10.);
#1693=VECTOR('',#6032,9.99999999999998);
#1694=VECTOR('',#6033,10.);
#1695=VECTOR('',#6036,10.);
#1696=VECTOR('',#6037,10.);
#1697=VECTOR('',#6038,10.);
#1698=VECTOR('',#6041,10.);
#1699=VECTOR('',#6042,10.);
#1700=VECTOR('',#6043,10.);
#1701=VECTOR('',#6048,10.);
#1702=VECTOR('',#6055,10.);
#1703=VECTOR('',#6060,10.);
#1704=VECTOR('',#6061,10.);
#1705=VECTOR('',#6062,10.);
#1706=VECTOR('',#6065,10.);
#1707=VECTOR('',#6066,10.);
#1708=VECTOR('',#6067,10.);
#1709=VECTOR('',#6070,10.);
#1710=VECTOR('',#6071,10.);
#1711=VECTOR('',#6072,10.);
#1712=VECTOR('',#6077,10.);
#1713=VECTOR('',#6082,10.);
#1714=VECTOR('',#6083,10.);
#1715=VECTOR('',#6084,10.);
#1716=VECTOR('',#6087,10.);
#1717=VECTOR('',#6088,10.);
#1718=VECTOR('',#6089,10.);
#1719=VECTOR('',#6092,10.);
#1720=VECTOR('',#6093,10.);
#1721=VECTOR('',#6096,10.);
#1722=VECTOR('',#6097,10.);
#1723=VECTOR('',#6098,10.);
#1724=VECTOR('',#6101,10.);
#1725=VECTOR('',#6102,10.);
#1726=VECTOR('',#6103,10.);
#1727=VECTOR('',#6106,10.);
#1728=VECTOR('',#6107,10.);
#1729=VECTOR('',#6108,10.);
#1730=VECTOR('',#6113,10.);
#1731=VECTOR('',#6118,10.);
#1732=VECTOR('',#6119,10.);
#1733=VECTOR('',#6120,10.);
#1734=VECTOR('',#6123,10.);
#1735=VECTOR('',#6124,10.);
#1736=VECTOR('',#6125,10.);
#1737=VECTOR('',#6128,10.);
#1738=VECTOR('',#6129,10.);
#1739=VECTOR('',#6132,9.99999999999998);
#1740=VECTOR('',#6133,10.);
#1741=VECTOR('',#6134,9.99999999999998);
#1742=VECTOR('',#6135,10.);
#1743=VECTOR('',#6138,9.99999999999998);
#1744=VECTOR('',#6139,10.);
#1745=VECTOR('',#6140,9.99999999999998);
#1746=VECTOR('',#6141,10.);
#1747=VECTOR('',#6146,10.);
#1748=VECTOR('',#6153,10.);
#1749=VECTOR('',#6160,10.);
#1750=VECTOR('',#6167,10.);
#1751=VECTOR('',#6172,9.99999999999999);
#1752=VECTOR('',#6173,9.99999999999999);
#1753=VECTOR('',#6176,9.99999999999999);
#1754=VECTOR('',#6177,10.);
#1755=VECTOR('',#6178,9.99999999999999);
#1756=VECTOR('',#6179,10.);
#1757=VECTOR('',#6184,10.);
#1758=VECTOR('',#6191,10.);
#1759=VECTOR('',#6196,10.);
#1760=VECTOR('',#6197,10.);
#1761=VECTOR('',#6198,10.);
#1762=VECTOR('',#6199,10.);
#1763=VECTOR('',#6202,10.);
#1764=VECTOR('',#6203,10.);
#1765=VECTOR('',#6204,10.);
#1766=VECTOR('',#6205,10.);
#1767=VECTOR('',#6210,10.);
#1768=VECTOR('',#6217,10.);
#1769=VECTOR('',#6224,10.);
#1770=VECTOR('',#6231,10.);
#1771=VECTOR('',#6236,10.);
#1772=VECTOR('',#6237,10.);
#1773=VECTOR('',#6238,10.);
#1774=VECTOR('',#6239,10.);
#1775=VECTOR('',#6242,10.);
#1776=VECTOR('',#6243,10.);
#1777=VECTOR('',#6244,10.);
#1778=VECTOR('',#6245,10.);
#1779=VECTOR('',#6250,10.);
#1780=VECTOR('',#6257,10.);
#1781=VECTOR('',#6264,10.);
#1782=VECTOR('',#6271,10.);
#1783=VECTOR('',#6276,10.);
#1784=VECTOR('',#6277,10.);
#1785=VECTOR('',#6280,10.);
#1786=VECTOR('',#6281,10.);
#1787=VECTOR('',#6282,10.);
#1788=VECTOR('',#6283,10.);
#1789=VECTOR('',#6288,10.);
#1790=VECTOR('',#6295,10.);
#1791=VECTOR('',#6300,10.);
#1792=VECTOR('',#6301,10.);
#1793=VECTOR('',#6304,10.);
#1794=VECTOR('',#6305,10.);
#1795=VECTOR('',#6308,9.99999999999998);
#1796=VECTOR('',#6309,9.99999999999998);
#1797=VECTOR('',#6312,9.99999999999998);
#1798=VECTOR('',#6313,10.);
#1799=VECTOR('',#6314,9.99999999999998);
#1800=VECTOR('',#6315,10.);
#1801=VECTOR('',#6320,10.);
#1802=VECTOR('',#6327,10.);
#1803=VECTOR('',#6332,10.);
#1804=VECTOR('',#6333,10.);
#1805=VECTOR('',#6336,10.);
#1806=VECTOR('',#6337,10.);
#1807=VECTOR('',#6340,9.99999999999998);
#1808=VECTOR('',#6341,10.);
#1809=VECTOR('',#6342,9.99999999999998);
#1810=VECTOR('',#6343,10.);
#1811=VECTOR('',#6346,10.);
#1812=VECTOR('',#6347,10.);
#1813=VECTOR('',#6348,10.);
#1814=VECTOR('',#6351,10.);
#1815=VECTOR('',#6352,10.);
#1816=VECTOR('',#6353,10.);
#1817=VECTOR('',#6358,10.);
#1818=VECTOR('',#6365,10.);
#1819=VECTOR('',#6370,10.);
#1820=VECTOR('',#6371,10.);
#1821=VECTOR('',#6372,10.);
#1822=VECTOR('',#6375,10.);
#1823=VECTOR('',#6376,10.);
#1824=VECTOR('',#6377,10.);
#1825=VECTOR('',#6380,10.);
#1826=VECTOR('',#6381,10.);
#1827=VECTOR('',#6382,10.);
#1828=VECTOR('',#6387,10.);
#1829=VECTOR('',#6392,10.);
#1830=VECTOR('',#6393,10.);
#1831=VECTOR('',#6394,10.);
#1832=VECTOR('',#6395,10.);
#1833=VECTOR('',#6398,10.);
#1834=VECTOR('',#6399,9.99999999999999);
#1835=VECTOR('',#6400,10.);
#1836=VECTOR('',#6403,10.);
#1837=VECTOR('',#6404,10.);
#1838=VECTOR('',#6405,10.);
#1839=VECTOR('',#6410,10.);
#1840=VECTOR('',#6417,10.);
#1841=VECTOR('',#6422,10.);
#1842=VECTOR('',#6423,10.);
#1843=VECTOR('',#6424,10.);
#1844=VECTOR('',#6425,10.);
#1845=VECTOR('',#6428,10.);
#1846=VECTOR('',#6429,10.);
#1847=VECTOR('',#6430,10.);
#1848=VECTOR('',#6433,10.);
#1849=VECTOR('',#6434,10.);
#1850=VECTOR('',#6435,10.);
#1851=VECTOR('',#6440,10.);
#1852=VECTOR('',#6447,10.);
#1853=VECTOR('',#6452,10.);
#1854=VECTOR('',#6453,10.);
#1855=VECTOR('',#6454,10.);
#1856=VECTOR('',#6457,10.);
#1857=VECTOR('',#6458,10.);
#1858=VECTOR('',#6459,10.);
#1859=VECTOR('',#6462,10.);
#1860=VECTOR('',#6463,10.);
#1861=VECTOR('',#6466,10.);
#1862=VECTOR('',#6467,10.);
#1863=VECTOR('',#6468,10.);
#1864=VECTOR('',#6471,10.);
#1865=VECTOR('',#6472,10.);
#1866=VECTOR('',#6473,10.);
#1867=VECTOR('',#6476,10.);
#1868=VECTOR('',#6477,10.);
#1869=VECTOR('',#6480,10.);
#1870=VECTOR('',#6481,10.);
#1871=VECTOR('',#6482,10.);
#1872=VECTOR('',#6485,10.);
#1873=VECTOR('',#6486,9.99999999999999);
#1874=VECTOR('',#6487,10.);
#1875=VECTOR('',#6490,10.);
#1876=VECTOR('',#6491,10.);
#1877=VECTOR('',#6494,10.);
#1878=VECTOR('',#6495,10.);
#1879=VECTOR('',#6496,10.);
#1880=VECTOR('',#6499,10.);
#1881=VECTOR('',#6500,10.);
#1882=VECTOR('',#6501,10.);
#1883=VECTOR('',#6504,10.);
#1884=VECTOR('',#6505,10.);
#1885=VECTOR('',#6506,10.);
#1886=VECTOR('',#6511,10.);
#1887=VECTOR('',#6516,9.99999999999999);
#1888=VECTOR('',#6517,9.99999999999999);
#1889=VECTOR('',#6520,9.99999999999999);
#1890=VECTOR('',#6521,10.);
#1891=VECTOR('',#6522,9.99999999999999);
#1892=VECTOR('',#6523,10.);
#1893=VECTOR('',#6528,10.);
#1894=VECTOR('',#6535,10.);
#1895=VECTOR('',#6540,10.);
#1896=VECTOR('',#6541,10.);
#1897=VECTOR('',#6542,10.);
#1898=VECTOR('',#6543,10.);
#1899=VECTOR('',#6546,10.);
#1900=VECTOR('',#6547,10.);
#1901=VECTOR('',#6552,10.);
#1902=VECTOR('',#6559,10.);
#1903=VECTOR('',#6564,10.);
#1904=VECTOR('',#6565,10.);
#1905=VECTOR('',#6568,10.);
#1906=VECTOR('',#6569,10.);
#1907=VECTOR('',#6572,10.);
#1908=VECTOR('',#6573,10.);
#1909=VECTOR('',#6574,10.);
#1910=VECTOR('',#6575,10.);
#1911=VECTOR('',#6578,10.);
#1912=VECTOR('',#6579,10.);
#1913=VECTOR('',#6580,10.);
#1914=VECTOR('',#6583,10.);
#1915=VECTOR('',#6584,10.);
#1916=VECTOR('',#6585,10.);
#1917=VECTOR('',#6590,10.);
#1918=VECTOR('',#6597,10.);
#1919=VECTOR('',#6602,10.);
#1920=VECTOR('',#6603,10.);
#1921=VECTOR('',#6604,10.);
#1922=VECTOR('',#6607,10.);
#1923=VECTOR('',#6608,10.);
#1924=VECTOR('',#6609,10.);
#1925=VECTOR('',#6612,10.);
#1926=VECTOR('',#6613,10.);
#1927=VECTOR('',#6614,10.);
#1928=VECTOR('',#6619,10.);
#1929=VECTOR('',#6624,10.);
#1930=VECTOR('',#6625,10.);
#1931=VECTOR('',#6626,10.);
#1932=VECTOR('',#6627,10.);
#1933=VECTOR('',#6630,10.);
#1934=VECTOR('',#6631,10.);
#1935=VECTOR('',#6632,10.);
#1936=VECTOR('',#6635,10.);
#1937=VECTOR('',#6636,10.);
#1938=VECTOR('',#6637,10.);
#1939=VECTOR('',#6642,10.);
#1940=VECTOR('',#6649,10.);
#1941=VECTOR('',#6654,10.);
#1942=VECTOR('',#6655,10.);
#1943=VECTOR('',#6656,10.);
#1944=VECTOR('',#6659,10.);
#1945=VECTOR('',#6660,10.);
#1946=VECTOR('',#6661,10.);
#1947=VECTOR('',#6664,10.);
#1948=VECTOR('',#6665,10.);
#1949=VECTOR('',#6666,10.);
#1950=VECTOR('',#6671,10.);
#1951=VECTOR('',#6676,10.);
#1952=VECTOR('',#6677,10.);
#1953=VECTOR('',#6678,10.);
#1954=VECTOR('',#6681,10.);
#1955=VECTOR('',#6682,10.);
#1956=VECTOR('',#6683,10.);
#1957=VECTOR('',#6686,10.);
#1958=VECTOR('',#6687,10.);
#1959=VECTOR('',#6688,10.);
#1960=VECTOR('',#6693,10.);
#1961=VECTOR('',#6698,10.);
#1962=VECTOR('',#6699,10.);
#1963=VECTOR('',#6700,10.);
#1964=VECTOR('',#6703,10.);
#1965=VECTOR('',#6704,10.);
#1966=VECTOR('',#6705,10.);
#1967=VECTOR('',#6708,10.);
#1968=VECTOR('',#6709,10.);
#1969=VECTOR('',#6712,10.);
#1970=VECTOR('',#6713,10.);
#1971=VECTOR('',#6714,10.);
#1972=VECTOR('',#6717,9.99999999999999);
#1973=VECTOR('',#6718,9.99999999999999);
#1974=VECTOR('',#6719,10.);
#1975=VECTOR('',#6722,10.);
#1976=VECTOR('',#6723,10.);
#1977=VECTOR('',#6726,10.);
#1978=VECTOR('',#6727,10.);
#1979=VECTOR('',#6728,10.);
#1980=VECTOR('',#6731,10.);
#1981=VECTOR('',#6732,10.);
#1982=VECTOR('',#6733,10.);
#1983=VECTOR('',#6736,10.);
#1984=VECTOR('',#6737,10.);
#1985=VECTOR('',#6740,10.);
#1986=VECTOR('',#6741,10.);
#1987=VECTOR('',#6744,10.);
#1988=VECTOR('',#6745,10.);
#1989=VECTOR('',#6750,1.99137169252308);
#1990=VECTOR('',#6763,1.26938918348039);
#1991=VECTOR('',#6768,10.);
#1992=VECTOR('',#6769,10.);
#1993=VECTOR('',#6770,10.);
#1994=VECTOR('',#6771,10.);
#1995=VECTOR('',#6774,10.);
#1996=VECTOR('',#6775,10.);
#1997=VECTOR('',#6776,10.);
#1998=VECTOR('',#6779,10.);
#1999=VECTOR('',#6780,10.);
#2000=VECTOR('',#6781,10.);
#2001=VECTOR('',#6784,10.);
#2002=VECTOR('',#6785,10.);
#2003=VECTOR('',#6794,10.);
#2004=VECTOR('',#6795,10.);
#2005=VECTOR('',#6796,10.);
#2006=VECTOR('',#6797,10.);
#2007=VECTOR('',#6800,10.);
#2008=VECTOR('',#6801,10.);
#2009=VECTOR('',#6802,10.);
#2010=VECTOR('',#6803,10.);
#2011=VECTOR('',#6812,10.);
#2012=VECTOR('',#6813,10.);
#2013=VECTOR('',#6814,10.);
#2014=VECTOR('',#6815,10.);
#2015=VECTOR('',#6818,10.);
#2016=VECTOR('',#6819,10.);
#2017=VECTOR('',#6820,10.);
#2018=VECTOR('',#6825,1.26938918348039);
#2019=VECTOR('',#6830,10.);
#2020=VECTOR('',#6831,10.);
#2021=VECTOR('',#6832,10.);
#2022=VECTOR('',#6841,10.);
#2023=VECTOR('',#6842,10.);
#2024=VECTOR('',#6843,10.);
#2025=VECTOR('',#6860,2.00038918348039);
#2026=VECTOR('',#6877,10.);
#2027=VECTOR('',#6878,10.);
#2028=VECTOR('',#6883,10.);
#2029=VECTOR('',#6890,10.);
#2030=VECTOR('',#6909,1.99137169252308);
#2031=VECTOR('',#6916,1.99137169252308);
#2032=VECTOR('',#6929,4.8);
#2033=VECTOR('',#6936,4.872);
#2034=VECTOR('',#6945,4.8);
#2035=VECTOR('',#6950,4.8);
#2036=VECTOR('',#6965,6.);
#2037=VECTOR('',#6974,4.845);
#2038=VECTOR('',#6989,3.1184375);
#2039=VECTOR('',#6996,3.1184375);
#2040=VECTOR('',#7009,3.272);
#2041=VECTOR('',#7022,3.1184375);
#2042=VECTOR('',#7027,3.0734375);
#2043=VECTOR('',#7040,2.);
#2044=VECTOR('',#7061,3.2);
#2045=VECTOR('',#7076,4.36638040039984);
#2046=VECTOR('',#7095,4.57071796769724);
#2047=VECTOR('',#7114,4.62071796769724);
#2048=VECTOR('',#7133,4.27977786002139);
#2049=VECTOR('',#7148,3.2);
#2050=VECTOR('',#7163,4.36638040039984);
#2051=VECTOR('',#7182,4.57071796769724);
#2052=VECTOR('',#7201,4.62071796769724);
#2053=VECTOR('',#7220,4.27977786002139);
#2054=VERTEX_POINT('',#7250);
#2055=VERTEX_POINT('',#7251);
#2056=VERTEX_POINT('',#7253);
#2057=VERTEX_POINT('',#7255);
#2058=VERTEX_POINT('',#7259);
#2059=VERTEX_POINT('',#7261);
#2060=VERTEX_POINT('',#7265);
#2061=VERTEX_POINT('',#7267);
#2062=VERTEX_POINT('',#7271);
#2063=VERTEX_POINT('',#7273);
#2064=VERTEX_POINT('',#7277);
#2065=VERTEX_POINT('',#7279);
#2066=VERTEX_POINT('',#7283);
#2067=VERTEX_POINT('',#7284);
#2068=VERTEX_POINT('',#7286);
#2069=VERTEX_POINT('',#7288);
#2070=VERTEX_POINT('',#7292);
#2071=VERTEX_POINT('',#7294);
#2072=VERTEX_POINT('',#7298);
#2073=VERTEX_POINT('',#7300);
#2074=VERTEX_POINT('',#7304);
#2075=VERTEX_POINT('',#7306);
#2076=VERTEX_POINT('',#7310);
#2077=VERTEX_POINT('',#7312);
#2078=VERTEX_POINT('',#7316);
#2079=VERTEX_POINT('',#7318);
#2080=VERTEX_POINT('',#7322);
#2081=VERTEX_POINT('',#7324);
#2082=VERTEX_POINT('',#7328);
#2083=VERTEX_POINT('',#7330);
#2084=VERTEX_POINT('',#7334);
#2085=VERTEX_POINT('',#7336);
#2086=VERTEX_POINT('',#7340);
#2087=VERTEX_POINT('',#7341);
#2088=VERTEX_POINT('',#7343);
#2089=VERTEX_POINT('',#7345);
#2090=VERTEX_POINT('',#7349);
#2091=VERTEX_POINT('',#7351);
#2092=VERTEX_POINT('',#7355);
#2093=VERTEX_POINT('',#7357);
#2094=VERTEX_POINT('',#7361);
#2095=VERTEX_POINT('',#7363);
#2096=VERTEX_POINT('',#7367);
#2097=VERTEX_POINT('',#7369);
#2098=VERTEX_POINT('',#7373);
#2099=VERTEX_POINT('',#7375);
#2100=VERTEX_POINT('',#7379);
#2101=VERTEX_POINT('',#7381);
#2102=VERTEX_POINT('',#7388);
#2103=VERTEX_POINT('',#7390);
#2104=VERTEX_POINT('',#7394);
#2105=VERTEX_POINT('',#7396);
#2106=VERTEX_POINT('',#7400);
#2107=VERTEX_POINT('',#7402);
#2108=VERTEX_POINT('',#7406);
#2109=VERTEX_POINT('',#7408);
#2110=VERTEX_POINT('',#7412);
#2111=VERTEX_POINT('',#7413);
#2112=VERTEX_POINT('',#7415);
#2113=VERTEX_POINT('',#7417);
#2114=VERTEX_POINT('',#7421);
#2115=VERTEX_POINT('',#7423);
#2116=VERTEX_POINT('',#7430);
#2117=VERTEX_POINT('',#7432);
#2118=VERTEX_POINT('',#7436);
#2119=VERTEX_POINT('',#7438);
#2120=VERTEX_POINT('',#7442);
#2121=VERTEX_POINT('',#7444);
#2122=VERTEX_POINT('',#7451);
#2123=VERTEX_POINT('',#7452);
#2124=VERTEX_POINT('',#7454);
#2125=VERTEX_POINT('',#7456);
#2126=VERTEX_POINT('',#7460);
#2127=VERTEX_POINT('',#7461);
#2128=VERTEX_POINT('',#7463);
#2129=VERTEX_POINT('',#7465);
#2130=VERTEX_POINT('',#7469);
#2131=VERTEX_POINT('',#7471);
#2132=VERTEX_POINT('',#7475);
#2133=VERTEX_POINT('',#7477);
#2134=VERTEX_POINT('',#7481);
#2135=VERTEX_POINT('',#7483);
#2136=VERTEX_POINT('',#7487);
#2137=VERTEX_POINT('',#7489);
#2138=VERTEX_POINT('',#7496);
#2139=VERTEX_POINT('',#7497);
#2140=VERTEX_POINT('',#7499);
#2141=VERTEX_POINT('',#7501);
#2142=VERTEX_POINT('',#7505);
#2143=VERTEX_POINT('',#7507);
#2144=VERTEX_POINT('',#7511);
#2145=VERTEX_POINT('',#7513);
#2146=VERTEX_POINT('',#7517);
#2147=VERTEX_POINT('',#7518);
#2148=VERTEX_POINT('',#7520);
#2149=VERTEX_POINT('',#7522);
#2150=VERTEX_POINT('',#7529);
#2151=VERTEX_POINT('',#7531);
#2152=VERTEX_POINT('',#7535);
#2153=VERTEX_POINT('',#7537);
#2154=VERTEX_POINT('',#7541);
#2155=VERTEX_POINT('',#7542);
#2156=VERTEX_POINT('',#7544);
#2157=VERTEX_POINT('',#7546);
#2158=VERTEX_POINT('',#7550);
#2159=VERTEX_POINT('',#7552);
#2160=VERTEX_POINT('',#7556);
#2161=VERTEX_POINT('',#7558);
#2162=VERTEX_POINT('',#7562);
#2163=VERTEX_POINT('',#7564);
#2164=VERTEX_POINT('',#7568);
#2165=VERTEX_POINT('',#7570);
#2166=VERTEX_POINT('',#7574);
#2167=VERTEX_POINT('',#7575);
#2168=VERTEX_POINT('',#7577);
#2169=VERTEX_POINT('',#7579);
#2170=VERTEX_POINT('',#7583);
#2171=VERTEX_POINT('',#7585);
#2172=VERTEX_POINT('',#7589);
#2173=VERTEX_POINT('',#7591);
#2174=VERTEX_POINT('',#7595);
#2175=VERTEX_POINT('',#7597);
#2176=VERTEX_POINT('',#7601);
#2177=VERTEX_POINT('',#7603);
#2178=VERTEX_POINT('',#7607);
#2179=VERTEX_POINT('',#7609);
#2180=VERTEX_POINT('',#7613);
#2181=VERTEX_POINT('',#7615);
#2182=VERTEX_POINT('',#7619);
#2183=VERTEX_POINT('',#7621);
#2184=VERTEX_POINT('',#7625);
#2185=VERTEX_POINT('',#7627);
#2186=VERTEX_POINT('',#7631);
#2187=VERTEX_POINT('',#7633);
#2188=VERTEX_POINT('',#7637);
#2189=VERTEX_POINT('',#7639);
#2190=VERTEX_POINT('',#7646);
#2191=VERTEX_POINT('',#7648);
#2192=VERTEX_POINT('',#7652);
#2193=VERTEX_POINT('',#7654);
#2194=VERTEX_POINT('',#7658);
#2195=VERTEX_POINT('',#7660);
#2196=VERTEX_POINT('',#7664);
#2197=VERTEX_POINT('',#7666);
#2198=VERTEX_POINT('',#7670);
#2199=VERTEX_POINT('',#7672);
#2200=VERTEX_POINT('',#7676);
#2201=VERTEX_POINT('',#7678);
#2202=VERTEX_POINT('',#7685);
#2203=VERTEX_POINT('',#7686);
#2204=VERTEX_POINT('',#7688);
#2205=VERTEX_POINT('',#7690);
#2206=VERTEX_POINT('',#7694);
#2207=VERTEX_POINT('',#7695);
#2208=VERTEX_POINT('',#7697);
#2209=VERTEX_POINT('',#7699);
#2210=VERTEX_POINT('',#7703);
#2211=VERTEX_POINT('',#7705);
#2212=VERTEX_POINT('',#7709);
#2213=VERTEX_POINT('',#7711);
#2214=VERTEX_POINT('',#7715);
#2215=VERTEX_POINT('',#7717);
#2216=VERTEX_POINT('',#7721);
#2217=VERTEX_POINT('',#7723);
#2218=VERTEX_POINT('',#7730);
#2219=VERTEX_POINT('',#7731);
#2220=VERTEX_POINT('',#7733);
#2221=VERTEX_POINT('',#7735);
#2222=VERTEX_POINT('',#7739);
#2223=VERTEX_POINT('',#7741);
#2224=VERTEX_POINT('',#7745);
#2225=VERTEX_POINT('',#7747);
#2226=VERTEX_POINT('',#7751);
#2227=VERTEX_POINT('',#7752);
#2228=VERTEX_POINT('',#7754);
#2229=VERTEX_POINT('',#7756);
#2230=VERTEX_POINT('',#7760);
#2231=VERTEX_POINT('',#7761);
#2232=VERTEX_POINT('',#7763);
#2233=VERTEX_POINT('',#7765);
#2234=VERTEX_POINT('',#7769);
#2235=VERTEX_POINT('',#7771);
#2236=VERTEX_POINT('',#7775);
#2237=VERTEX_POINT('',#7777);
#2238=VERTEX_POINT('',#7781);
#2239=VERTEX_POINT('',#7783);
#2240=VERTEX_POINT('',#7787);
#2241=VERTEX_POINT('',#7789);
#2242=VERTEX_POINT('',#7793);
#2243=VERTEX_POINT('',#7794);
#2244=VERTEX_POINT('',#7796);
#2245=VERTEX_POINT('',#7798);
#2246=VERTEX_POINT('',#7802);
#2247=VERTEX_POINT('',#7803);
#2248=VERTEX_POINT('',#7805);
#2249=VERTEX_POINT('',#7807);
#2250=VERTEX_POINT('',#7811);
#2251=VERTEX_POINT('',#7813);
#2252=VERTEX_POINT('',#7817);
#2253=VERTEX_POINT('',#7819);
#2254=VERTEX_POINT('',#7823);
#2255=VERTEX_POINT('',#7825);
#2256=VERTEX_POINT('',#7829);
#2257=VERTEX_POINT('',#7831);
#2258=VERTEX_POINT('',#7838);
#2259=VERTEX_POINT('',#7839);
#2260=VERTEX_POINT('',#7841);
#2261=VERTEX_POINT('',#7843);
#2262=VERTEX_POINT('',#7847);
#2263=VERTEX_POINT('',#7849);
#2264=VERTEX_POINT('',#7853);
#2265=VERTEX_POINT('',#7855);
#2266=VERTEX_POINT('',#7868);
#2267=VERTEX_POINT('',#7869);
#2268=VERTEX_POINT('',#7871);
#2269=VERTEX_POINT('',#7873);
#2270=VERTEX_POINT('',#7877);
#2271=VERTEX_POINT('',#7879);
#2272=VERTEX_POINT('',#7883);
#2273=VERTEX_POINT('',#7885);
#2274=VERTEX_POINT('',#7895);
#2275=VERTEX_POINT('',#7896);
#2276=VERTEX_POINT('',#7898);
#2277=VERTEX_POINT('',#7900);
#2278=VERTEX_POINT('',#7904);
#2279=VERTEX_POINT('',#7906);
#2280=VERTEX_POINT('',#7910);
#2281=VERTEX_POINT('',#7912);
#2282=VERTEX_POINT('',#7916);
#2283=VERTEX_POINT('',#7918);
#2284=VERTEX_POINT('',#7922);
#2285=VERTEX_POINT('',#7924);
#2286=VERTEX_POINT('',#7928);
#2287=VERTEX_POINT('',#7930);
#2288=VERTEX_POINT('',#7934);
#2289=VERTEX_POINT('',#7936);
#2290=VERTEX_POINT('',#7940);
#2291=VERTEX_POINT('',#7942);
#2292=VERTEX_POINT('',#7946);
#2293=VERTEX_POINT('',#7948);
#2294=VERTEX_POINT('',#7952);
#2295=VERTEX_POINT('',#7953);
#2296=VERTEX_POINT('',#7955);
#2297=VERTEX_POINT('',#7957);
#2298=VERTEX_POINT('',#7961);
#2299=VERTEX_POINT('',#7963);
#2300=VERTEX_POINT('',#7967);
#2301=VERTEX_POINT('',#7969);
#2302=VERTEX_POINT('',#7973);
#2303=VERTEX_POINT('',#7975);
#2304=VERTEX_POINT('',#7979);
#2305=VERTEX_POINT('',#7981);
#2306=VERTEX_POINT('',#7985);
#2307=VERTEX_POINT('',#7986);
#2308=VERTEX_POINT('',#7988);
#2309=VERTEX_POINT('',#7990);
#2310=VERTEX_POINT('',#7994);
#2311=VERTEX_POINT('',#7996);
#2312=VERTEX_POINT('',#8000);
#2313=VERTEX_POINT('',#8002);
#2314=VERTEX_POINT('',#8006);
#2315=VERTEX_POINT('',#8008);
#2316=VERTEX_POINT('',#8012);
#2317=VERTEX_POINT('',#8014);
#2318=VERTEX_POINT('',#8018);
#2319=VERTEX_POINT('',#8020);
#2320=VERTEX_POINT('',#8024);
#2321=VERTEX_POINT('',#8026);
#2322=VERTEX_POINT('',#8033);
#2323=VERTEX_POINT('',#8035);
#2324=VERTEX_POINT('',#8039);
#2325=VERTEX_POINT('',#8041);
#2326=VERTEX_POINT('',#8048);
#2327=VERTEX_POINT('',#8050);
#2328=VERTEX_POINT('',#8054);
#2329=VERTEX_POINT('',#8056);
#2330=VERTEX_POINT('',#8063);
#2331=VERTEX_POINT('',#8065);
#2332=VERTEX_POINT('',#8069);
#2333=VERTEX_POINT('',#8071);
#2334=VERTEX_POINT('',#8075);
#2335=VERTEX_POINT('',#8077);
#2336=VERTEX_POINT('',#8081);
#2337=VERTEX_POINT('',#8083);
#2338=VERTEX_POINT('',#8090);
#2339=VERTEX_POINT('',#8091);
#2340=VERTEX_POINT('',#8093);
#2341=VERTEX_POINT('',#8095);
#2342=VERTEX_POINT('',#8099);
#2343=VERTEX_POINT('',#8101);
#2344=VERTEX_POINT('',#8105);
#2345=VERTEX_POINT('',#8107);
#2346=VERTEX_POINT('',#8111);
#2347=VERTEX_POINT('',#8112);
#2348=VERTEX_POINT('',#8114);
#2349=VERTEX_POINT('',#8116);
#2350=VERTEX_POINT('',#8123);
#2351=VERTEX_POINT('',#8125);
#2352=VERTEX_POINT('',#8129);
#2353=VERTEX_POINT('',#8131);
#2354=VERTEX_POINT('',#8141);
#2355=VERTEX_POINT('',#8142);
#2356=VERTEX_POINT('',#8144);
#2357=VERTEX_POINT('',#8146);
#2358=VERTEX_POINT('',#8150);
#2359=VERTEX_POINT('',#8152);
#2360=VERTEX_POINT('',#8156);
#2361=VERTEX_POINT('',#8158);
#2362=VERTEX_POINT('',#8162);
#2363=VERTEX_POINT('',#8164);
#2364=VERTEX_POINT('',#8168);
#2365=VERTEX_POINT('',#8170);
#2366=VERTEX_POINT('',#8174);
#2367=VERTEX_POINT('',#8176);
#2368=VERTEX_POINT('',#8180);
#2369=VERTEX_POINT('',#8182);
#2370=VERTEX_POINT('',#8186);
#2371=VERTEX_POINT('',#8188);
#2372=VERTEX_POINT('',#8192);
#2373=VERTEX_POINT('',#8194);
#2374=VERTEX_POINT('',#8198);
#2375=VERTEX_POINT('',#8199);
#2376=VERTEX_POINT('',#8201);
#2377=VERTEX_POINT('',#8203);
#2378=VERTEX_POINT('',#8207);
#2379=VERTEX_POINT('',#8209);
#2380=VERTEX_POINT('',#8213);
#2381=VERTEX_POINT('',#8215);
#2382=VERTEX_POINT('',#8219);
#2383=VERTEX_POINT('',#8221);
#2384=VERTEX_POINT('',#8225);
#2385=VERTEX_POINT('',#8227);
#2386=VERTEX_POINT('',#8231);
#2387=VERTEX_POINT('',#8233);
#2388=VERTEX_POINT('',#8237);
#2389=VERTEX_POINT('',#8239);
#2390=VERTEX_POINT('',#8243);
#2391=VERTEX_POINT('',#8245);
#2392=VERTEX_POINT('',#8249);
#2393=VERTEX_POINT('',#8251);
#2394=VERTEX_POINT('',#8255);
#2395=VERTEX_POINT('',#8257);
#2396=VERTEX_POINT('',#8261);
#2397=VERTEX_POINT('',#8263);
#2398=VERTEX_POINT('',#8267);
#2399=VERTEX_POINT('',#8269);
#2400=VERTEX_POINT('',#8273);
#2401=VERTEX_POINT('',#8275);
#2402=VERTEX_POINT('',#8279);
#2403=VERTEX_POINT('',#8281);
#2404=VERTEX_POINT('',#8285);
#2405=VERTEX_POINT('',#8287);
#2406=VERTEX_POINT('',#8294);
#2407=VERTEX_POINT('',#8296);
#2408=VERTEX_POINT('',#8300);
#2409=VERTEX_POINT('',#8302);
#2410=VERTEX_POINT('',#8309);
#2411=VERTEX_POINT('',#8311);
#2412=VERTEX_POINT('',#8315);
#2413=VERTEX_POINT('',#8317);
#2414=VERTEX_POINT('',#8330);
#2415=VERTEX_POINT('',#8332);
#2416=VERTEX_POINT('',#8339);
#2417=VERTEX_POINT('',#8341);
#2418=VERTEX_POINT('',#8345);
#2419=VERTEX_POINT('',#8346);
#2420=VERTEX_POINT('',#8348);
#2421=VERTEX_POINT('',#8350);
#2422=VERTEX_POINT('',#8354);
#2423=VERTEX_POINT('',#8356);
#2424=VERTEX_POINT('',#8360);
#2425=VERTEX_POINT('',#8362);
#2426=VERTEX_POINT('',#8372);
#2427=VERTEX_POINT('',#8373);
#2428=VERTEX_POINT('',#8375);
#2429=VERTEX_POINT('',#8377);
#2430=VERTEX_POINT('',#8381);
#2431=VERTEX_POINT('',#8382);
#2432=VERTEX_POINT('',#8384);
#2433=VERTEX_POINT('',#8386);
#2434=VERTEX_POINT('',#8393);
#2435=VERTEX_POINT('',#8394);
#2436=VERTEX_POINT('',#8396);
#2437=VERTEX_POINT('',#8398);
#2438=VERTEX_POINT('',#8402);
#2439=VERTEX_POINT('',#8404);
#2440=VERTEX_POINT('',#8408);
#2441=VERTEX_POINT('',#8410);
#2442=VERTEX_POINT('',#8414);
#2443=VERTEX_POINT('',#8416);
#2444=VERTEX_POINT('',#8423);
#2445=VERTEX_POINT('',#8425);
#2446=VERTEX_POINT('',#8435);
#2447=VERTEX_POINT('',#8437);
#2448=VERTEX_POINT('',#8444);
#2449=VERTEX_POINT('',#8446);
#2450=VERTEX_POINT('',#8449);
#2451=VERTEX_POINT('',#8450);
#2452=VERTEX_POINT('',#8461);
#2453=VERTEX_POINT('',#8463);
#2454=VERTEX_POINT('',#8476);
#2455=VERTEX_POINT('',#8477);
#2456=VERTEX_POINT('',#8479);
#2457=VERTEX_POINT('',#8484);
#2458=VERTEX_POINT('',#8495);
#2459=VERTEX_POINT('',#8514);
#2460=VERTEX_POINT('',#8520);
#2461=VERTEX_POINT('',#8522);
#2462=VERTEX_POINT('',#8529);
#2463=VERTEX_POINT('',#8531);
#2464=VERTEX_POINT('',#8535);
#2465=VERTEX_POINT('',#8537);
#2466=VERTEX_POINT('',#8541);
#2467=VERTEX_POINT('',#8542);
#2468=VERTEX_POINT('',#8545);
#2469=VERTEX_POINT('',#8549);
#2470=VERTEX_POINT('',#8553);
#2471=VERTEX_POINT('',#8555);
#2472=VERTEX_POINT('',#8559);
#2473=VERTEX_POINT('',#8563);
#2474=VERTEX_POINT('',#8567);
#2475=VERTEX_POINT('',#8575);
#2476=VERTEX_POINT('',#8576);
#2477=VERTEX_POINT('',#8578);
#2478=VERTEX_POINT('',#8583);
#2479=VERTEX_POINT('',#8587);
#2480=VERTEX_POINT('',#8591);
#2481=VERTEX_POINT('',#8593);
#2482=VERTEX_POINT('',#8597);
#2483=VERTEX_POINT('',#8599);
#2484=VERTEX_POINT('',#8603);
#2485=VERTEX_POINT('',#8607);
#2486=VERTEX_POINT('',#8611);
#2487=VERTEX_POINT('',#8613);
#2488=VERTEX_POINT('',#8617);
#2489=VERTEX_POINT('',#8621);
#2490=VERTEX_POINT('',#8629);
#2491=VERTEX_POINT('',#8631);
#2492=VERTEX_POINT('',#8635);
#2493=VERTEX_POINT('',#8637);
#2494=VERTEX_POINT('',#8641);
#2495=VERTEX_POINT('',#8645);
#2496=VERTEX_POINT('',#8649);
#2497=VERTEX_POINT('',#8651);
#2498=VERTEX_POINT('',#8655);
#2499=VERTEX_POINT('',#8659);
#2500=VERTEX_POINT('',#8663);
#2501=VERTEX_POINT('',#8665);
#2502=VERTEX_POINT('',#8669);
#2503=VERTEX_POINT('',#8673);
#2504=VERTEX_POINT('',#8677);
#2505=VERTEX_POINT('',#8679);
#2506=VERTEX_POINT('',#8683);
#2507=VERTEX_POINT('',#8692);
#2508=VERTEX_POINT('',#8694);
#2509=VERTEX_POINT('',#8698);
#2510=VERTEX_POINT('',#8700);
#2511=VERTEX_POINT('',#8704);
#2512=VERTEX_POINT('',#8708);
#2513=VERTEX_POINT('',#8712);
#2514=VERTEX_POINT('',#8714);
#2515=VERTEX_POINT('',#8718);
#2516=VERTEX_POINT('',#8722);
#2517=VERTEX_POINT('',#8726);
#2518=VERTEX_POINT('',#8728);
#2519=VERTEX_POINT('',#8732);
#2520=VERTEX_POINT('',#8736);
#2521=VERTEX_POINT('',#8740);
#2522=VERTEX_POINT('',#8742);
#2523=VERTEX_POINT('',#8746);
#2524=EDGE_CURVE('',#2054,#2055,#1084,.F.);
#2525=EDGE_CURVE('',#2056,#2055,#1085,.T.);
#2526=EDGE_CURVE('',#2057,#2056,#1086,.T.);
#2527=EDGE_CURVE('',#2054,#2057,#1087,.T.);
#2528=EDGE_CURVE('',#2054,#2058,#1088,.T.);
#2529=EDGE_CURVE('',#2059,#2057,#1089,.T.);
#2530=EDGE_CURVE('',#2058,#2059,#1090,.T.);
#2531=EDGE_CURVE('',#2058,#2060,#1091,.T.);
#2532=EDGE_CURVE('',#2061,#2059,#1092,.T.);
#2533=EDGE_CURVE('',#2060,#2061,#1093,.T.);
#2534=EDGE_CURVE('',#2062,#2055,#169,.T.);
#2535=EDGE_CURVE('',#2062,#2063,#1094,.T.);
#2536=EDGE_CURVE('',#2056,#2063,#170,.T.);
#2537=EDGE_CURVE('',#2064,#2061,#171,.T.);
#2538=EDGE_CURVE('',#2064,#2065,#1095,.T.);
#2539=EDGE_CURVE('',#2060,#2065,#172,.T.);
#2540=EDGE_CURVE('',#2066,#2067,#1096,.F.);
#2541=EDGE_CURVE('',#2068,#2067,#1097,.T.);
#2542=EDGE_CURVE('',#2069,#2068,#1098,.T.);
#2543=EDGE_CURVE('',#2066,#2069,#1099,.T.);
#2544=EDGE_CURVE('',#2066,#2070,#1100,.T.);
#2545=EDGE_CURVE('',#2071,#2069,#1101,.T.);
#2546=EDGE_CURVE('',#2070,#2071,#1102,.T.);
#2547=EDGE_CURVE('',#2070,#2072,#1103,.T.);
#2548=EDGE_CURVE('',#2073,#2071,#1104,.T.);
#2549=EDGE_CURVE('',#2072,#2073,#1105,.T.);
#2550=EDGE_CURVE('',#2074,#2067,#173,.T.);
#2551=EDGE_CURVE('',#2074,#2075,#1106,.T.);
#2552=EDGE_CURVE('',#2068,#2075,#174,.T.);
#2553=EDGE_CURVE('',#2076,#2073,#175,.T.);
#2554=EDGE_CURVE('',#2076,#2077,#1107,.T.);
#2555=EDGE_CURVE('',#2072,#2077,#176,.T.);
#2556=EDGE_CURVE('',#2078,#2065,#1108,.F.);
#2557=EDGE_CURVE('',#2079,#2064,#1109,.T.);
#2558=EDGE_CURVE('',#2078,#2079,#1110,.T.);
#2559=EDGE_CURVE('',#2078,#2080,#1111,.T.);
#2560=EDGE_CURVE('',#2081,#2079,#1112,.T.);
#2561=EDGE_CURVE('',#2080,#2081,#1113,.T.);
#2562=EDGE_CURVE('',#2080,#2082,#1114,.T.);
#2563=EDGE_CURVE('',#2083,#2081,#1115,.T.);
#2564=EDGE_CURVE('',#2082,#2083,#1116,.T.);
#2565=EDGE_CURVE('',#2084,#2083,#177,.T.);
#2566=EDGE_CURVE('',#2084,#2085,#1117,.T.);
#2567=EDGE_CURVE('',#2082,#2085,#178,.T.);
#2568=EDGE_CURVE('',#2086,#2087,#1118,.F.);
#2569=EDGE_CURVE('',#2088,#2087,#1119,.T.);
#2570=EDGE_CURVE('',#2089,#2088,#1120,.T.);
#2571=EDGE_CURVE('',#2086,#2089,#1121,.T.);
#2572=EDGE_CURVE('',#2086,#2090,#1122,.T.);
#2573=EDGE_CURVE('',#2091,#2089,#1123,.T.);
#2574=EDGE_CURVE('',#2090,#2091,#1124,.T.);
#2575=EDGE_CURVE('',#2090,#2092,#1125,.T.);
#2576=EDGE_CURVE('',#2093,#2091,#1126,.T.);
#2577=EDGE_CURVE('',#2092,#2093,#1127,.T.);
#2578=EDGE_CURVE('',#2094,#2087,#179,.T.);
#2579=EDGE_CURVE('',#2094,#2095,#1128,.T.);
#2580=EDGE_CURVE('',#2088,#2095,#180,.T.);
#2581=EDGE_CURVE('',#2096,#2093,#181,.T.);
#2582=EDGE_CURVE('',#2096,#2097,#1129,.T.);
#2583=EDGE_CURVE('',#2092,#2097,#182,.T.);
#2584=EDGE_CURVE('',#2098,#2085,#1130,.F.);
#2585=EDGE_CURVE('',#2099,#2084,#1131,.T.);
#2586=EDGE_CURVE('',#2098,#2099,#1132,.T.);
#2587=EDGE_CURVE('',#2098,#2100,#1133,.T.);
#2588=EDGE_CURVE('',#2101,#2099,#1134,.T.);
#2589=EDGE_CURVE('',#2100,#2101,#1135,.T.);
#2590=EDGE_CURVE('',#2100,#2074,#1136,.T.);
#2591=EDGE_CURVE('',#2075,#2101,#1137,.T.);
#2592=EDGE_CURVE('',#2102,#2077,#1138,.F.);
#2593=EDGE_CURVE('',#2103,#2076,#1139,.T.);
#2594=EDGE_CURVE('',#2102,#2103,#1140,.T.);
#2595=EDGE_CURVE('',#2102,#2104,#1141,.T.);
#2596=EDGE_CURVE('',#2105,#2103,#1142,.T.);
#2597=EDGE_CURVE('',#2104,#2105,#1143,.T.);
#2598=EDGE_CURVE('',#2104,#2106,#1144,.T.);
#2599=EDGE_CURVE('',#2107,#2105,#1145,.T.);
#2600=EDGE_CURVE('',#2106,#2107,#1146,.T.);
#2601=EDGE_CURVE('',#2108,#2107,#183,.T.);
#2602=EDGE_CURVE('',#2108,#2109,#1147,.T.);
#2603=EDGE_CURVE('',#2106,#2109,#184,.T.);
#2604=EDGE_CURVE('',#2110,#2111,#1148,.F.);
#2605=EDGE_CURVE('',#2112,#2111,#1149,.T.);
#2606=EDGE_CURVE('',#2113,#2112,#1150,.T.);
#2607=EDGE_CURVE('',#2110,#2113,#1151,.T.);
#2608=EDGE_CURVE('',#2110,#2114,#1152,.T.);
#2609=EDGE_CURVE('',#2115,#2113,#1153,.T.);
#2610=EDGE_CURVE('',#2114,#2115,#1154,.T.);
#2611=EDGE_CURVE('',#2114,#2062,#1155,.T.);
#2612=EDGE_CURVE('',#2063,#2115,#1156,.T.);
#2613=EDGE_CURVE('',#2116,#2111,#185,.T.);
#2614=EDGE_CURVE('',#2116,#2117,#1157,.T.);
#2615=EDGE_CURVE('',#2112,#2117,#186,.T.);
#2616=EDGE_CURVE('',#2118,#2109,#1158,.F.);
#2617=EDGE_CURVE('',#2119,#2108,#1159,.T.);
#2618=EDGE_CURVE('',#2118,#2119,#1160,.T.);
#2619=EDGE_CURVE('',#2118,#2120,#1161,.T.);
#2620=EDGE_CURVE('',#2121,#2119,#1162,.T.);
#2621=EDGE_CURVE('',#2120,#2121,#1163,.T.);
#2622=EDGE_CURVE('',#2120,#2094,#1164,.T.);
#2623=EDGE_CURVE('',#2095,#2121,#1165,.T.);
#2624=EDGE_CURVE('',#2122,#2123,#1166,.T.);
#2625=EDGE_CURVE('',#2124,#2122,#1167,.T.);
#2626=EDGE_CURVE('',#2125,#2124,#1168,.T.);
#2627=EDGE_CURVE('',#2123,#2125,#1169,.T.);
#2628=EDGE_CURVE('',#2126,#2127,#1170,.T.);
#2629=EDGE_CURVE('',#2128,#2126,#1171,.T.);
#2630=EDGE_CURVE('',#2129,#2128,#1172,.T.);
#2631=EDGE_CURVE('',#2127,#2129,#1173,.T.);
#2632=EDGE_CURVE('',#2130,#2122,#187,.T.);
#2633=EDGE_CURVE('',#2130,#2131,#1174,.T.);
#2634=EDGE_CURVE('',#2124,#2131,#188,.T.);
#2635=EDGE_CURVE('',#2132,#2129,#189,.T.);
#2636=EDGE_CURVE('',#2132,#2133,#1175,.T.);
#2637=EDGE_CURVE('',#2127,#2133,#190,.T.);
#2638=EDGE_CURVE('',#2134,#2125,#191,.T.);
#2639=EDGE_CURVE('',#2134,#2135,#1176,.T.);
#2640=EDGE_CURVE('',#2123,#2135,#192,.T.);
#2641=EDGE_CURVE('',#2136,#2126,#193,.T.);
#2642=EDGE_CURVE('',#2136,#2137,#1177,.T.);
#2643=EDGE_CURVE('',#2128,#2137,#194,.T.);
#2644=EDGE_CURVE('',#2133,#2136,#1178,.T.);
#2645=EDGE_CURVE('',#2137,#2132,#1179,.T.);
#2646=EDGE_CURVE('',#2138,#2139,#1180,.T.);
#2647=EDGE_CURVE('',#2140,#2138,#1181,.T.);
#2648=EDGE_CURVE('',#2141,#2140,#1182,.T.);
#2649=EDGE_CURVE('',#2139,#2141,#1183,.T.);
#2650=EDGE_CURVE('',#2142,#2141,#195,.T.);
#2651=EDGE_CURVE('',#2142,#2143,#1184,.T.);
#2652=EDGE_CURVE('',#2139,#2143,#196,.T.);
#2653=EDGE_CURVE('',#2144,#2138,#197,.T.);
#2654=EDGE_CURVE('',#2144,#2145,#1185,.T.);
#2655=EDGE_CURVE('',#2140,#2145,#198,.T.);
#2656=EDGE_CURVE('',#2146,#2147,#1186,.T.);
#2657=EDGE_CURVE('',#2148,#2146,#1187,.T.);
#2658=EDGE_CURVE('',#2149,#2148,#1188,.T.);
#2659=EDGE_CURVE('',#2147,#2149,#1189,.T.);
#2660=EDGE_CURVE('',#2135,#2130,#1190,.T.);
#2661=EDGE_CURVE('',#2131,#2134,#1191,.T.);
#2662=EDGE_CURVE('',#2150,#2146,#199,.T.);
#2663=EDGE_CURVE('',#2150,#2151,#1192,.T.);
#2664=EDGE_CURVE('',#2148,#2151,#200,.T.);
#2665=EDGE_CURVE('',#2152,#2149,#201,.T.);
#2666=EDGE_CURVE('',#2152,#2153,#1193,.T.);
#2667=EDGE_CURVE('',#2147,#2153,#202,.T.);
#2668=EDGE_CURVE('',#2154,#2155,#1194,.F.);
#2669=EDGE_CURVE('',#2156,#2155,#1195,.T.);
#2670=EDGE_CURVE('',#2157,#2156,#1196,.T.);
#2671=EDGE_CURVE('',#2154,#2157,#1197,.T.);
#2672=EDGE_CURVE('',#2154,#2158,#1198,.T.);
#2673=EDGE_CURVE('',#2159,#2157,#1199,.T.);
#2674=EDGE_CURVE('',#2158,#2159,#1200,.T.);
#2675=EDGE_CURVE('',#2158,#2160,#1201,.T.);
#2676=EDGE_CURVE('',#2161,#2159,#1202,.T.);
#2677=EDGE_CURVE('',#2160,#2161,#1203,.T.);
#2678=EDGE_CURVE('',#2162,#2155,#203,.T.);
#2679=EDGE_CURVE('',#2162,#2163,#1204,.T.);
#2680=EDGE_CURVE('',#2156,#2163,#204,.T.);
#2681=EDGE_CURVE('',#2164,#2161,#205,.T.);
#2682=EDGE_CURVE('',#2164,#2165,#1205,.T.);
#2683=EDGE_CURVE('',#2160,#2165,#206,.T.);
#2684=EDGE_CURVE('',#2166,#2167,#1206,.F.);
#2685=EDGE_CURVE('',#2168,#2167,#1207,.T.);
#2686=EDGE_CURVE('',#2169,#2168,#1208,.T.);
#2687=EDGE_CURVE('',#2166,#2169,#1209,.T.);
#2688=EDGE_CURVE('',#2166,#2170,#1210,.T.);
#2689=EDGE_CURVE('',#2171,#2169,#1211,.T.);
#2690=EDGE_CURVE('',#2170,#2171,#1212,.T.);
#2691=EDGE_CURVE('',#2170,#2172,#1213,.T.);
#2692=EDGE_CURVE('',#2173,#2171,#1214,.T.);
#2693=EDGE_CURVE('',#2172,#2173,#1215,.T.);
#2694=EDGE_CURVE('',#2174,#2167,#207,.T.);
#2695=EDGE_CURVE('',#2174,#2175,#1216,.T.);
#2696=EDGE_CURVE('',#2168,#2175,#208,.T.);
#2697=EDGE_CURVE('',#2176,#2173,#209,.T.);
#2698=EDGE_CURVE('',#2176,#2177,#1217,.T.);
#2699=EDGE_CURVE('',#2172,#2177,#210,.T.);
#2700=EDGE_CURVE('',#2178,#2177,#1218,.F.);
#2701=EDGE_CURVE('',#2179,#2176,#1219,.T.);
#2702=EDGE_CURVE('',#2178,#2179,#1220,.T.);
#2703=EDGE_CURVE('',#2178,#2180,#1221,.T.);
#2704=EDGE_CURVE('',#2181,#2179,#1222,.T.);
#2705=EDGE_CURVE('',#2180,#2181,#1223,.T.);
#2706=EDGE_CURVE('',#2180,#2182,#1224,.T.);
#2707=EDGE_CURVE('',#2183,#2181,#1225,.T.);
#2708=EDGE_CURVE('',#2182,#2183,#1226,.T.);
#2709=EDGE_CURVE('',#2184,#2183,#211,.T.);
#2710=EDGE_CURVE('',#2184,#2185,#1227,.T.);
#2711=EDGE_CURVE('',#2182,#2185,#212,.T.);
#2712=EDGE_CURVE('',#2186,#2185,#1228,.F.);
#2713=EDGE_CURVE('',#2187,#2184,#1229,.T.);
#2714=EDGE_CURVE('',#2186,#2187,#1230,.T.);
#2715=EDGE_CURVE('',#2186,#2188,#1231,.T.);
#2716=EDGE_CURVE('',#2189,#2187,#1232,.T.);
#2717=EDGE_CURVE('',#2188,#2189,#1233,.T.);
#2718=EDGE_CURVE('',#2188,#2162,#1234,.T.);
#2719=EDGE_CURVE('',#2163,#2189,#1235,.T.);
#2720=EDGE_CURVE('',#2190,#2165,#1236,.F.);
#2721=EDGE_CURVE('',#2191,#2164,#1237,.T.);
#2722=EDGE_CURVE('',#2190,#2191,#1238,.T.);
#2723=EDGE_CURVE('',#2190,#2192,#1239,.T.);
#2724=EDGE_CURVE('',#2193,#2191,#1240,.T.);
#2725=EDGE_CURVE('',#2192,#2193,#1241,.T.);
#2726=EDGE_CURVE('',#2192,#2194,#1242,.T.);
#2727=EDGE_CURVE('',#2195,#2193,#1243,.T.);
#2728=EDGE_CURVE('',#2194,#2195,#1244,.T.);
#2729=EDGE_CURVE('',#2196,#2195,#213,.T.);
#2730=EDGE_CURVE('',#2196,#2197,#1245,.T.);
#2731=EDGE_CURVE('',#2194,#2197,#214,.T.);
#2732=EDGE_CURVE('',#2198,#2197,#1246,.F.);
#2733=EDGE_CURVE('',#2199,#2196,#1247,.T.);
#2734=EDGE_CURVE('',#2198,#2199,#1248,.T.);
#2735=EDGE_CURVE('',#2198,#2200,#1249,.T.);
#2736=EDGE_CURVE('',#2201,#2199,#1250,.T.);
#2737=EDGE_CURVE('',#2200,#2201,#1251,.T.);
#2738=EDGE_CURVE('',#2200,#2116,#1252,.T.);
#2739=EDGE_CURVE('',#2117,#2201,#1253,.T.);
#2740=EDGE_CURVE('',#2202,#2203,#1254,.T.);
#2741=EDGE_CURVE('',#2204,#2202,#1255,.T.);
#2742=EDGE_CURVE('',#2205,#2204,#1256,.T.);
#2743=EDGE_CURVE('',#2203,#2205,#1257,.T.);
#2744=EDGE_CURVE('',#2206,#2207,#1258,.T.);
#2745=EDGE_CURVE('',#2208,#2206,#1259,.T.);
#2746=EDGE_CURVE('',#2209,#2208,#1260,.T.);
#2747=EDGE_CURVE('',#2207,#2209,#1261,.T.);
#2748=EDGE_CURVE('',#2210,#2202,#215,.T.);
#2749=EDGE_CURVE('',#2210,#2211,#1262,.T.);
#2750=EDGE_CURVE('',#2204,#2211,#216,.T.);
#2751=EDGE_CURVE('',#2212,#2209,#217,.T.);
#2752=EDGE_CURVE('',#2212,#2213,#1263,.T.);
#2753=EDGE_CURVE('',#2207,#2213,#218,.T.);
#2754=EDGE_CURVE('',#2214,#2205,#219,.T.);
#2755=EDGE_CURVE('',#2214,#2215,#1264,.T.);
#2756=EDGE_CURVE('',#2203,#2215,#220,.T.);
#2757=EDGE_CURVE('',#2216,#2206,#221,.T.);
#2758=EDGE_CURVE('',#2216,#2217,#1265,.T.);
#2759=EDGE_CURVE('',#2208,#2217,#222,.T.);
#2760=EDGE_CURVE('',#2213,#2216,#1266,.T.);
#2761=EDGE_CURVE('',#2217,#2212,#1267,.T.);
#2762=EDGE_CURVE('',#2218,#2219,#1268,.T.);
#2763=EDGE_CURVE('',#2220,#2218,#1269,.T.);
#2764=EDGE_CURVE('',#2221,#2220,#1270,.T.);
#2765=EDGE_CURVE('',#2219,#2221,#1271,.T.);
#2766=EDGE_CURVE('',#2222,#2221,#223,.T.);
#2767=EDGE_CURVE('',#2222,#2223,#1272,.T.);
#2768=EDGE_CURVE('',#2219,#2223,#224,.T.);
#2769=EDGE_CURVE('',#2224,#2218,#225,.T.);
#2770=EDGE_CURVE('',#2224,#2225,#1273,.T.);
#2771=EDGE_CURVE('',#2220,#2225,#226,.T.);
#2772=EDGE_CURVE('',#2226,#2227,#1274,.T.);
#2773=EDGE_CURVE('',#2228,#2226,#1275,.T.);
#2774=EDGE_CURVE('',#2229,#2228,#1276,.T.);
#2775=EDGE_CURVE('',#2227,#2229,#1277,.T.);
#2776=EDGE_CURVE('',#2230,#2231,#1278,.T.);
#2777=EDGE_CURVE('',#2232,#2230,#1279,.T.);
#2778=EDGE_CURVE('',#2233,#2232,#1280,.T.);
#2779=EDGE_CURVE('',#2231,#2233,#1281,.T.);
#2780=EDGE_CURVE('',#2234,#2226,#227,.T.);
#2781=EDGE_CURVE('',#2234,#2235,#1282,.T.);
#2782=EDGE_CURVE('',#2228,#2235,#228,.T.);
#2783=EDGE_CURVE('',#2236,#2233,#229,.T.);
#2784=EDGE_CURVE('',#2236,#2237,#1283,.T.);
#2785=EDGE_CURVE('',#2231,#2237,#230,.T.);
#2786=EDGE_CURVE('',#2238,#2229,#231,.T.);
#2787=EDGE_CURVE('',#2238,#2239,#1284,.T.);
#2788=EDGE_CURVE('',#2227,#2239,#232,.T.);
#2789=EDGE_CURVE('',#2240,#2230,#233,.T.);
#2790=EDGE_CURVE('',#2240,#2241,#1285,.T.);
#2791=EDGE_CURVE('',#2232,#2241,#234,.T.);
#2792=EDGE_CURVE('',#2242,#2243,#1286,.T.);
#2793=EDGE_CURVE('',#2244,#2242,#1287,.T.);
#2794=EDGE_CURVE('',#2245,#2244,#1288,.T.);
#2795=EDGE_CURVE('',#2243,#2245,#1289,.T.);
#2796=EDGE_CURVE('',#2246,#2247,#1290,.T.);
#2797=EDGE_CURVE('',#2248,#2246,#1291,.T.);
#2798=EDGE_CURVE('',#2249,#2248,#1292,.T.);
#2799=EDGE_CURVE('',#2247,#2249,#1293,.T.);
#2800=EDGE_CURVE('',#2250,#2242,#235,.T.);
#2801=EDGE_CURVE('',#2250,#2251,#1294,.T.);
#2802=EDGE_CURVE('',#2244,#2251,#236,.T.);
#2803=EDGE_CURVE('',#2252,#2249,#237,.T.);
#2804=EDGE_CURVE('',#2252,#2253,#1295,.T.);
#2805=EDGE_CURVE('',#2247,#2253,#238,.T.);
#2806=EDGE_CURVE('',#2254,#2245,#239,.T.);
#2807=EDGE_CURVE('',#2254,#2255,#1296,.T.);
#2808=EDGE_CURVE('',#2243,#2255,#240,.T.);
#2809=EDGE_CURVE('',#2256,#2246,#241,.T.);
#2810=EDGE_CURVE('',#2256,#2257,#1297,.T.);
#2811=EDGE_CURVE('',#2248,#2257,#242,.T.);
#2812=EDGE_CURVE('',#2223,#2224,#1298,.T.);
#2813=EDGE_CURVE('',#2225,#2222,#1299,.T.);
#2814=EDGE_CURVE('',#2258,#2259,#1300,.T.);
#2815=EDGE_CURVE('',#2260,#2258,#1301,.T.);
#2816=EDGE_CURVE('',#2261,#2260,#1302,.T.);
#2817=EDGE_CURVE('',#2259,#2261,#1303,.T.);
#2818=EDGE_CURVE('',#2262,#2261,#243,.T.);
#2819=EDGE_CURVE('',#2262,#2263,#1304,.T.);
#2820=EDGE_CURVE('',#2259,#2263,#244,.T.);
#2821=EDGE_CURVE('',#2264,#2258,#245,.T.);
#2822=EDGE_CURVE('',#2264,#2265,#1305,.T.);
#2823=EDGE_CURVE('',#2260,#2265,#246,.T.);
#2824=EDGE_CURVE('',#2253,#2256,#1306,.T.);
#2825=EDGE_CURVE('',#2257,#2252,#1307,.T.);
#2826=EDGE_CURVE('',#2239,#2234,#1308,.T.);
#2827=EDGE_CURVE('',#2235,#2238,#1309,.T.);
#2828=EDGE_CURVE('',#2263,#2264,#1310,.T.);
#2829=EDGE_CURVE('',#2265,#2262,#1311,.T.);
#2830=EDGE_CURVE('',#2266,#2267,#1312,.T.);
#2831=EDGE_CURVE('',#2268,#2266,#1313,.T.);
#2832=EDGE_CURVE('',#2269,#2268,#1314,.T.);
#2833=EDGE_CURVE('',#2267,#2269,#1315,.T.);
#2834=EDGE_CURVE('',#2270,#2269,#247,.T.);
#2835=EDGE_CURVE('',#2270,#2271,#1316,.T.);
#2836=EDGE_CURVE('',#2267,#2271,#248,.T.);
#2837=EDGE_CURVE('',#2272,#2266,#249,.T.);
#2838=EDGE_CURVE('',#2272,#2273,#1317,.T.);
#2839=EDGE_CURVE('',#2268,#2273,#250,.T.);
#2840=EDGE_CURVE('',#2237,#2240,#1318,.T.);
#2841=EDGE_CURVE('',#2241,#2236,#1319,.T.);
#2842=EDGE_CURVE('',#2215,#2210,#1320,.T.);
#2843=EDGE_CURVE('',#2211,#2214,#1321,.T.);
#2844=EDGE_CURVE('',#2274,#2275,#1322,.F.);
#2845=EDGE_CURVE('',#2276,#2275,#1323,.T.);
#2846=EDGE_CURVE('',#2277,#2276,#1324,.T.);
#2847=EDGE_CURVE('',#2274,#2277,#1325,.T.);
#2848=EDGE_CURVE('',#2274,#2278,#1326,.T.);
#2849=EDGE_CURVE('',#2279,#2277,#1327,.T.);
#2850=EDGE_CURVE('',#2278,#2279,#1328,.T.);
#2851=EDGE_CURVE('',#2278,#2280,#1329,.T.);
#2852=EDGE_CURVE('',#2281,#2279,#1330,.T.);
#2853=EDGE_CURVE('',#2280,#2281,#1331,.T.);
#2854=EDGE_CURVE('',#2282,#2275,#251,.T.);
#2855=EDGE_CURVE('',#2282,#2283,#1332,.T.);
#2856=EDGE_CURVE('',#2276,#2283,#252,.T.);
#2857=EDGE_CURVE('',#2284,#2281,#253,.T.);
#2858=EDGE_CURVE('',#2284,#2285,#1333,.T.);
#2859=EDGE_CURVE('',#2280,#2285,#254,.T.);
#2860=EDGE_CURVE('',#2286,#2285,#1334,.F.);
#2861=EDGE_CURVE('',#2287,#2284,#1335,.T.);
#2862=EDGE_CURVE('',#2286,#2287,#1336,.T.);
#2863=EDGE_CURVE('',#2286,#2288,#1337,.T.);
#2864=EDGE_CURVE('',#2289,#2287,#1338,.T.);
#2865=EDGE_CURVE('',#2288,#2289,#1339,.T.);
#2866=EDGE_CURVE('',#2288,#2290,#1340,.T.);
#2867=EDGE_CURVE('',#2291,#2289,#1341,.T.);
#2868=EDGE_CURVE('',#2290,#2291,#1342,.T.);
#2869=EDGE_CURVE('',#2292,#2291,#255,.T.);
#2870=EDGE_CURVE('',#2292,#2293,#1343,.T.);
#2871=EDGE_CURVE('',#2290,#2293,#256,.T.);
#2872=EDGE_CURVE('',#2294,#2295,#1344,.F.);
#2873=EDGE_CURVE('',#2296,#2295,#1345,.T.);
#2874=EDGE_CURVE('',#2297,#2296,#1346,.T.);
#2875=EDGE_CURVE('',#2294,#2297,#1347,.T.);
#2876=EDGE_CURVE('',#2294,#2298,#1348,.T.);
#2877=EDGE_CURVE('',#2299,#2297,#1349,.T.);
#2878=EDGE_CURVE('',#2298,#2299,#1350,.T.);
#2879=EDGE_CURVE('',#2298,#2300,#1351,.T.);
#2880=EDGE_CURVE('',#2301,#2299,#1352,.T.);
#2881=EDGE_CURVE('',#2300,#2301,#1353,.T.);
#2882=EDGE_CURVE('',#2302,#2295,#257,.T.);
#2883=EDGE_CURVE('',#2302,#2303,#1354,.T.);
#2884=EDGE_CURVE('',#2296,#2303,#258,.T.);
#2885=EDGE_CURVE('',#2304,#2301,#259,.T.);
#2886=EDGE_CURVE('',#2304,#2305,#1355,.T.);
#2887=EDGE_CURVE('',#2300,#2305,#260,.T.);
#2888=EDGE_CURVE('',#2306,#2307,#1356,.F.);
#2889=EDGE_CURVE('',#2308,#2307,#1357,.T.);
#2890=EDGE_CURVE('',#2309,#2308,#1358,.T.);
#2891=EDGE_CURVE('',#2306,#2309,#1359,.T.);
#2892=EDGE_CURVE('',#2306,#2310,#1360,.T.);
#2893=EDGE_CURVE('',#2311,#2309,#1361,.T.);
#2894=EDGE_CURVE('',#2310,#2311,#1362,.T.);
#2895=EDGE_CURVE('',#2310,#2312,#1363,.T.);
#2896=EDGE_CURVE('',#2313,#2311,#1364,.T.);
#2897=EDGE_CURVE('',#2312,#2313,#1365,.T.);
#2898=EDGE_CURVE('',#2314,#2307,#261,.T.);
#2899=EDGE_CURVE('',#2314,#2315,#1366,.T.);
#2900=EDGE_CURVE('',#2308,#2315,#262,.T.);
#2901=EDGE_CURVE('',#2316,#2313,#263,.T.);
#2902=EDGE_CURVE('',#2316,#2317,#1367,.T.);
#2903=EDGE_CURVE('',#2312,#2317,#264,.T.);
#2904=EDGE_CURVE('',#2318,#2305,#1368,.F.);
#2905=EDGE_CURVE('',#2319,#2304,#1369,.T.);
#2906=EDGE_CURVE('',#2318,#2319,#1370,.T.);
#2907=EDGE_CURVE('',#2318,#2320,#1371,.T.);
#2908=EDGE_CURVE('',#2321,#2319,#1372,.T.);
#2909=EDGE_CURVE('',#2320,#2321,#1373,.T.);
#2910=EDGE_CURVE('',#2320,#2314,#1374,.T.);
#2911=EDGE_CURVE('',#2315,#2321,#1375,.T.);
#2912=EDGE_CURVE('',#2322,#2097,#1376,.F.);
#2913=EDGE_CURVE('',#2323,#2096,#1377,.T.);
#2914=EDGE_CURVE('',#2322,#2323,#1378,.T.);
#2915=EDGE_CURVE('',#2322,#2324,#1379,.T.);
#2916=EDGE_CURVE('',#2325,#2323,#1380,.T.);
#2917=EDGE_CURVE('',#2324,#2325,#1381,.T.);
#2918=EDGE_CURVE('',#2324,#2282,#1382,.T.);
#2919=EDGE_CURVE('',#2283,#2325,#1383,.T.);
#2920=EDGE_CURVE('',#2326,#2293,#1384,.F.);
#2921=EDGE_CURVE('',#2327,#2292,#1385,.T.);
#2922=EDGE_CURVE('',#2326,#2327,#1386,.T.);
#2923=EDGE_CURVE('',#2326,#2328,#1387,.T.);
#2924=EDGE_CURVE('',#2329,#2327,#1388,.T.);
#2925=EDGE_CURVE('',#2328,#2329,#1389,.T.);
#2926=EDGE_CURVE('',#2328,#2302,#1390,.T.);
#2927=EDGE_CURVE('',#2303,#2329,#1391,.T.);
#2928=EDGE_CURVE('',#2330,#2317,#1392,.F.);
#2929=EDGE_CURVE('',#2331,#2316,#1393,.T.);
#2930=EDGE_CURVE('',#2330,#2331,#1394,.T.);
#2931=EDGE_CURVE('',#2330,#2332,#1395,.T.);
#2932=EDGE_CURVE('',#2333,#2331,#1396,.T.);
#2933=EDGE_CURVE('',#2332,#2333,#1397,.T.);
#2934=EDGE_CURVE('',#2332,#2334,#1398,.T.);
#2935=EDGE_CURVE('',#2335,#2333,#1399,.T.);
#2936=EDGE_CURVE('',#2334,#2335,#1400,.T.);
#2937=EDGE_CURVE('',#2336,#2335,#265,.T.);
#2938=EDGE_CURVE('',#2336,#2337,#1401,.T.);
#2939=EDGE_CURVE('',#2334,#2337,#266,.T.);
#2940=EDGE_CURVE('',#2271,#2272,#1402,.T.);
#2941=EDGE_CURVE('',#2273,#2270,#1403,.T.);
#2942=EDGE_CURVE('',#2338,#2339,#1404,.T.);
#2943=EDGE_CURVE('',#2340,#2338,#1405,.T.);
#2944=EDGE_CURVE('',#2341,#2340,#1406,.T.);
#2945=EDGE_CURVE('',#2339,#2341,#1407,.T.);
#2946=EDGE_CURVE('',#2342,#2341,#267,.T.);
#2947=EDGE_CURVE('',#2342,#2343,#1408,.T.);
#2948=EDGE_CURVE('',#2339,#2343,#268,.T.);
#2949=EDGE_CURVE('',#2344,#2338,#269,.T.);
#2950=EDGE_CURVE('',#2344,#2345,#1409,.T.);
#2951=EDGE_CURVE('',#2340,#2345,#270,.T.);
#2952=EDGE_CURVE('',#2346,#2347,#1410,.T.);
#2953=EDGE_CURVE('',#2348,#2346,#1411,.T.);
#2954=EDGE_CURVE('',#2349,#2348,#1412,.T.);
#2955=EDGE_CURVE('',#2347,#2349,#1413,.T.);
#2956=EDGE_CURVE('',#2153,#2150,#1414,.T.);
#2957=EDGE_CURVE('',#2151,#2152,#1415,.T.);
#2958=EDGE_CURVE('',#2350,#2346,#271,.T.);
#2959=EDGE_CURVE('',#2350,#2351,#1416,.T.);
#2960=EDGE_CURVE('',#2348,#2351,#272,.T.);
#2961=EDGE_CURVE('',#2352,#2349,#273,.T.);
#2962=EDGE_CURVE('',#2352,#2353,#1417,.T.);
#2963=EDGE_CURVE('',#2347,#2353,#274,.T.);
#2964=EDGE_CURVE('',#2343,#2344,#1418,.T.);
#2965=EDGE_CURVE('',#2345,#2342,#1419,.T.);
#2966=EDGE_CURVE('',#2353,#2350,#1420,.T.);
#2967=EDGE_CURVE('',#2351,#2352,#1421,.T.);
#2968=EDGE_CURVE('',#2354,#2355,#1422,.F.);
#2969=EDGE_CURVE('',#2356,#2355,#1423,.T.);
#2970=EDGE_CURVE('',#2357,#2356,#1424,.T.);
#2971=EDGE_CURVE('',#2354,#2357,#1425,.T.);
#2972=EDGE_CURVE('',#2354,#2358,#1426,.T.);
#2973=EDGE_CURVE('',#2359,#2357,#1427,.T.);
#2974=EDGE_CURVE('',#2358,#2359,#1428,.T.);
#2975=EDGE_CURVE('',#2358,#2360,#1429,.T.);
#2976=EDGE_CURVE('',#2361,#2359,#1430,.T.);
#2977=EDGE_CURVE('',#2360,#2361,#1431,.T.);
#2978=EDGE_CURVE('',#2362,#2355,#275,.T.);
#2979=EDGE_CURVE('',#2362,#2363,#1432,.T.);
#2980=EDGE_CURVE('',#2356,#2363,#276,.T.);
#2981=EDGE_CURVE('',#2364,#2361,#277,.T.);
#2982=EDGE_CURVE('',#2364,#2365,#1433,.T.);
#2983=EDGE_CURVE('',#2360,#2365,#278,.T.);
#2984=EDGE_CURVE('',#2366,#2365,#1434,.F.);
#2985=EDGE_CURVE('',#2367,#2364,#1435,.T.);
#2986=EDGE_CURVE('',#2366,#2367,#1436,.T.);
#2987=EDGE_CURVE('',#2366,#2368,#1437,.T.);
#2988=EDGE_CURVE('',#2369,#2367,#1438,.T.);
#2989=EDGE_CURVE('',#2368,#2369,#1439,.T.);
#2990=EDGE_CURVE('',#2368,#2370,#1440,.T.);
#2991=EDGE_CURVE('',#2371,#2369,#1441,.T.);
#2992=EDGE_CURVE('',#2370,#2371,#1442,.T.);
#2993=EDGE_CURVE('',#2372,#2371,#279,.T.);
#2994=EDGE_CURVE('',#2372,#2373,#1443,.T.);
#2995=EDGE_CURVE('',#2370,#2373,#280,.T.);
#2996=EDGE_CURVE('',#2374,#2375,#1444,.F.);
#2997=EDGE_CURVE('',#2376,#2375,#1445,.T.);
#2998=EDGE_CURVE('',#2377,#2376,#1446,.T.);
#2999=EDGE_CURVE('',#2374,#2377,#1447,.T.);
#3000=EDGE_CURVE('',#2374,#2378,#1448,.T.);
#3001=EDGE_CURVE('',#2379,#2377,#1449,.T.);
#3002=EDGE_CURVE('',#2378,#2379,#1450,.T.);
#3003=EDGE_CURVE('',#2378,#2380,#1451,.T.);
#3004=EDGE_CURVE('',#2381,#2379,#1452,.T.);
#3005=EDGE_CURVE('',#2380,#2381,#1453,.T.);
#3006=EDGE_CURVE('',#2382,#2375,#281,.T.);
#3007=EDGE_CURVE('',#2382,#2383,#1454,.T.);
#3008=EDGE_CURVE('',#2376,#2383,#282,.T.);
#3009=EDGE_CURVE('',#2384,#2381,#283,.T.);
#3010=EDGE_CURVE('',#2384,#2385,#1455,.T.);
#3011=EDGE_CURVE('',#2380,#2385,#284,.T.);
#3012=EDGE_CURVE('',#2386,#2373,#1456,.F.);
#3013=EDGE_CURVE('',#2387,#2372,#1457,.T.);
#3014=EDGE_CURVE('',#2386,#2387,#1458,.T.);
#3015=EDGE_CURVE('',#2386,#2388,#1459,.T.);
#3016=EDGE_CURVE('',#2389,#2387,#1460,.T.);
#3017=EDGE_CURVE('',#2388,#2389,#1461,.T.);
#3018=EDGE_CURVE('',#2388,#2390,#1462,.T.);
#3019=EDGE_CURVE('',#2391,#2389,#1463,.T.);
#3020=EDGE_CURVE('',#2390,#2391,#1464,.T.);
#3021=EDGE_CURVE('',#2392,#2391,#285,.T.);
#3022=EDGE_CURVE('',#2392,#2393,#1465,.T.);
#3023=EDGE_CURVE('',#2390,#2393,#286,.T.);
#3024=EDGE_CURVE('',#2394,#2337,#1466,.F.);
#3025=EDGE_CURVE('',#2395,#2336,#1467,.T.);
#3026=EDGE_CURVE('',#2394,#2395,#1468,.T.);
#3027=EDGE_CURVE('',#2394,#2396,#1469,.T.);
#3028=EDGE_CURVE('',#2397,#2395,#1470,.T.);
#3029=EDGE_CURVE('',#2396,#2397,#1471,.T.);
#3030=EDGE_CURVE('',#2396,#2398,#1472,.T.);
#3031=EDGE_CURVE('',#2399,#2397,#1473,.T.);
#3032=EDGE_CURVE('',#2398,#2399,#1474,.T.);
#3033=EDGE_CURVE('',#2400,#2399,#287,.T.);
#3034=EDGE_CURVE('',#2400,#2401,#1475,.T.);
#3035=EDGE_CURVE('',#2398,#2401,#288,.T.);
#3036=EDGE_CURVE('',#2402,#2385,#1476,.F.);
#3037=EDGE_CURVE('',#2403,#2384,#1477,.T.);
#3038=EDGE_CURVE('',#2402,#2403,#1478,.T.);
#3039=EDGE_CURVE('',#2402,#2404,#1479,.T.);
#3040=EDGE_CURVE('',#2405,#2403,#1480,.T.);
#3041=EDGE_CURVE('',#2404,#2405,#1481,.T.);
#3042=EDGE_CURVE('',#2404,#2174,#1482,.T.);
#3043=EDGE_CURVE('',#2175,#2405,#1483,.T.);
#3044=EDGE_CURVE('',#2406,#2393,#1484,.F.);
#3045=EDGE_CURVE('',#2407,#2392,#1485,.T.);
#3046=EDGE_CURVE('',#2406,#2407,#1486,.T.);
#3047=EDGE_CURVE('',#2406,#2408,#1487,.T.);
#3048=EDGE_CURVE('',#2409,#2407,#1488,.T.);
#3049=EDGE_CURVE('',#2408,#2409,#1489,.T.);
#3050=EDGE_CURVE('',#2408,#2382,#1490,.T.);
#3051=EDGE_CURVE('',#2383,#2409,#1491,.T.);
#3052=EDGE_CURVE('',#2410,#2401,#1492,.F.);
#3053=EDGE_CURVE('',#2411,#2400,#1493,.T.);
#3054=EDGE_CURVE('',#2410,#2411,#1494,.T.);
#3055=EDGE_CURVE('',#2410,#2412,#1495,.T.);
#3056=EDGE_CURVE('',#2413,#2411,#1496,.T.);
#3057=EDGE_CURVE('',#2412,#2413,#1497,.T.);
#3058=EDGE_CURVE('',#2412,#2362,#1498,.T.);
#3059=EDGE_CURVE('',#2363,#2413,#1499,.T.);
#3060=EDGE_CURVE('',#2143,#2144,#1500,.T.);
#3061=EDGE_CURVE('',#2145,#2142,#1501,.T.);
#3062=EDGE_CURVE('',#2255,#2250,#1502,.T.);
#3063=EDGE_CURVE('',#2251,#2254,#1503,.T.);
#3064=EDGE_CURVE('',#2414,#2414,#289,.T.);
#3065=EDGE_CURVE('',#2414,#2415,#1504,.T.);
#3066=EDGE_CURVE('',#2415,#2415,#290,.T.);
#3067=EDGE_CURVE('',#2416,#2416,#291,.T.);
#3068=EDGE_CURVE('',#2416,#2417,#1505,.T.);
#3069=EDGE_CURVE('',#2417,#2417,#292,.T.);
#3070=EDGE_CURVE('',#2418,#2419,#1506,.T.);
#3071=EDGE_CURVE('',#2419,#2420,#1507,.T.);
#3072=EDGE_CURVE('',#2420,#2421,#1508,.T.);
#3073=EDGE_CURVE('',#2418,#2421,#1509,.T.);
#3074=EDGE_CURVE('',#2418,#2422,#1510,.T.);
#3075=EDGE_CURVE('',#2423,#2421,#1511,.T.);
#3076=EDGE_CURVE('',#2422,#2423,#1512,.T.);
#3077=EDGE_CURVE('',#2422,#2424,#1513,.T.);
#3078=EDGE_CURVE('',#2425,#2423,#1514,.T.);
#3079=EDGE_CURVE('',#2424,#2425,#1515,.T.);
#3080=EDGE_CURVE('',#2424,#2419,#1516,.T.);
#3081=EDGE_CURVE('',#2425,#2420,#1517,.T.);
#3082=EDGE_CURVE('',#2426,#2427,#1518,.T.);
#3083=EDGE_CURVE('',#2426,#2428,#1519,.T.);
#3084=EDGE_CURVE('',#2429,#2428,#1520,.T.);
#3085=EDGE_CURVE('',#2429,#2427,#1521,.T.);
#3086=EDGE_CURVE('',#2430,#2431,#1522,.T.);
#3087=EDGE_CURVE('',#2432,#2431,#1523,.T.);
#3088=EDGE_CURVE('',#2433,#2432,#1524,.T.);
#3089=EDGE_CURVE('',#2430,#2433,#1525,.T.);
#3090=EDGE_CURVE('',#2430,#2426,#293,.T.);
#3091=EDGE_CURVE('',#2428,#2433,#294,.T.);
#3092=EDGE_CURVE('',#2434,#2435,#1526,.T.);
#3093=EDGE_CURVE('',#2436,#2435,#1527,.T.);
#3094=EDGE_CURVE('',#2437,#2436,#1528,.T.);
#3095=EDGE_CURVE('',#2434,#2437,#1529,.T.);
#3096=EDGE_CURVE('',#2434,#2438,#1530,.T.);
#3097=EDGE_CURVE('',#2439,#2437,#1531,.T.);
#3098=EDGE_CURVE('',#2439,#2438,#1532,.T.);
#3099=EDGE_CURVE('',#2440,#2440,#295,.T.);
#3100=EDGE_CURVE('',#2440,#2441,#1533,.T.);
#3101=EDGE_CURVE('',#2441,#2441,#296,.T.);
#3102=EDGE_CURVE('',#2436,#2442,#1534,.T.);
#3103=EDGE_CURVE('',#2443,#2435,#1535,.T.);
#3104=EDGE_CURVE('',#2442,#2443,#1536,.T.);
#3105=EDGE_CURVE('',#2442,#2429,#297,.T.);
#3106=EDGE_CURVE('',#2427,#2443,#298,.T.);
#3107=EDGE_CURVE('',#2444,#2432,#1537,.F.);
#3108=EDGE_CURVE('',#2445,#2431,#1538,.T.);
#3109=EDGE_CURVE('',#2444,#2445,#1539,.T.);
#3110=EDGE_CURVE('',#2444,#2439,#299,.T.);
#3111=EDGE_CURVE('',#2438,#2445,#300,.T.);
#3112=EDGE_CURVE('',#2446,#2446,#301,.T.);
#3113=EDGE_CURVE('',#2446,#2447,#1540,.T.);
#3114=EDGE_CURVE('',#2447,#2447,#302,.T.);
#3115=EDGE_CURVE('',#2448,#2448,#303,.T.);
#3116=EDGE_CURVE('',#2449,#2449,#304,.T.);
#3117=EDGE_CURVE('',#2450,#2451,#76,.T.);
#3118=EDGE_CURVE('',#2452,#2450,#1541,.T.);
#3119=EDGE_CURVE('',#2453,#2452,#77,.T.);
#3120=EDGE_CURVE('',#2451,#2453,#1542,.T.);
#3121=EDGE_CURVE('',#2454,#2455,#305,.T.);
#3122=EDGE_CURVE('',#2454,#2456,#1543,.T.);
#3123=EDGE_CURVE('',#2452,#2456,#306,.T.);
#3124=EDGE_CURVE('',#2455,#2450,#307,.T.);
#3125=EDGE_CURVE('',#2457,#2454,#78,.T.);
#3126=EDGE_CURVE('',#2458,#2457,#1544,.T.);
#3127=EDGE_CURVE('',#2456,#2458,#79,.T.);
#3128=EDGE_CURVE('',#2451,#2453,#308,.T.);
#3129=EDGE_CURVE('',#2455,#2448,#309,.T.);
#3130=EDGE_CURVE('',#2458,#2457,#310,.T.);
#3131=EDGE_CURVE('',#2459,#2459,#311,.T.);
#3132=EDGE_CURVE('',#2449,#2459,#1545,.T.);
#3133=EDGE_CURVE('',#2460,#2460,#312,.T.);
#3134=EDGE_CURVE('',#2460,#2461,#1546,.T.);
#3135=EDGE_CURVE('',#2461,#2461,#313,.T.);
#3136=EDGE_CURVE('',#2462,#2462,#314,.T.);
#3137=EDGE_CURVE('',#2462,#2463,#1547,.T.);
#3138=EDGE_CURVE('',#2463,#2463,#315,.T.);
#3139=EDGE_CURVE('',#2464,#2464,#316,.T.);
#3140=EDGE_CURVE('',#2464,#2465,#1548,.T.);
#3141=EDGE_CURVE('',#2465,#2465,#317,.T.);
#3142=EDGE_CURVE('',#2466,#2467,#318,.T.);
#3143=EDGE_CURVE('',#2467,#2466,#319,.T.);
#3144=EDGE_CURVE('',#2467,#2468,#1549,.T.);
#3145=EDGE_CURVE('',#2468,#2468,#320,.T.);
#3146=EDGE_CURVE('',#2466,#2469,#1550,.T.);
#3147=EDGE_CURVE('',#2469,#2469,#321,.T.);
#3148=EDGE_CURVE('',#2470,#2470,#322,.T.);
#3149=EDGE_CURVE('',#2470,#2471,#323,.T.);
#3150=EDGE_CURVE('',#2471,#2471,#324,.T.);
#3151=EDGE_CURVE('',#2472,#2472,#325,.T.);
#3152=EDGE_CURVE('',#2472,#2470,#1551,.T.);
#3153=EDGE_CURVE('',#2473,#2473,#326,.T.);
#3154=EDGE_CURVE('',#2473,#2472,#327,.T.);
#3155=EDGE_CURVE('',#2463,#2474,#1552,.T.);
#3156=EDGE_CURVE('',#2474,#2474,#328,.T.);
#3157=EDGE_CURVE('',#2475,#2476,#329,.T.);
#3158=EDGE_CURVE('',#2476,#2477,#1553,.T.);
#3159=EDGE_CURVE('',#2477,#2477,#330,.T.);
#3160=EDGE_CURVE('',#2476,#2475,#331,.T.);
#3161=EDGE_CURVE('',#2475,#2478,#1554,.T.);
#3162=EDGE_CURVE('',#2478,#2478,#332,.T.);
#3163=EDGE_CURVE('',#2478,#2479,#333,.T.);
#3164=EDGE_CURVE('',#2479,#2479,#334,.T.);
#3165=EDGE_CURVE('',#2480,#2480,#335,.T.);
#3166=EDGE_CURVE('',#2480,#2481,#1555,.T.);
#3167=EDGE_CURVE('',#2481,#2481,#336,.T.);
#3168=EDGE_CURVE('',#2482,#2482,#337,.T.);
#3169=EDGE_CURVE('',#2482,#2483,#338,.T.);
#3170=EDGE_CURVE('',#2483,#2483,#339,.T.);
#3171=EDGE_CURVE('',#2483,#2484,#1556,.T.);
#3172=EDGE_CURVE('',#2484,#2484,#340,.T.);
#3173=EDGE_CURVE('',#2484,#2485,#1557,.T.);
#3174=EDGE_CURVE('',#2485,#2485,#341,.T.);
#3175=EDGE_CURVE('',#2486,#2486,#342,.T.);
#3176=EDGE_CURVE('',#2486,#2487,#343,.T.);
#3177=EDGE_CURVE('',#2487,#2487,#344,.T.);
#3178=EDGE_CURVE('',#2487,#2488,#1558,.T.);
#3179=EDGE_CURVE('',#2488,#2488,#345,.T.);
#3180=EDGE_CURVE('',#2488,#2489,#346,.T.);
#3181=EDGE_CURVE('',#2489,#2489,#347,.T.);
#3182=EDGE_CURVE('',#2490,#2490,#348,.T.);
#3183=EDGE_CURVE('',#2490,#2491,#1559,.T.);
#3184=EDGE_CURVE('',#2491,#2491,#349,.T.);
#3185=EDGE_CURVE('',#2492,#2492,#350,.T.);
#3186=EDGE_CURVE('',#2492,#2493,#351,.T.);
#3187=EDGE_CURVE('',#2493,#2493,#352,.T.);
#3188=EDGE_CURVE('',#2494,#2494,#353,.T.);
#3189=EDGE_CURVE('',#2494,#2492,#1560,.T.);
#3190=EDGE_CURVE('',#2495,#2495,#354,.T.);
#3191=EDGE_CURVE('',#2495,#2494,#355,.T.);
#3192=EDGE_CURVE('',#2496,#2496,#356,.T.);
#3193=EDGE_CURVE('',#2496,#2497,#357,.T.);
#3194=EDGE_CURVE('',#2497,#2497,#358,.T.);
#3195=EDGE_CURVE('',#2498,#2498,#359,.T.);
#3196=EDGE_CURVE('',#2498,#2496,#1561,.T.);
#3197=EDGE_CURVE('',#2499,#2499,#360,.T.);
#3198=EDGE_CURVE('',#2499,#2498,#361,.T.);
#3199=EDGE_CURVE('',#2500,#2500,#362,.T.);
#3200=EDGE_CURVE('',#2500,#2501,#363,.T.);
#3201=EDGE_CURVE('',#2501,#2501,#364,.T.);
#3202=EDGE_CURVE('',#2502,#2502,#365,.T.);
#3203=EDGE_CURVE('',#2502,#2500,#1562,.T.);
#3204=EDGE_CURVE('',#2503,#2503,#366,.T.);
#3205=EDGE_CURVE('',#2503,#2502,#367,.T.);
#3206=EDGE_CURVE('',#2504,#2504,#368,.T.);
#3207=EDGE_CURVE('',#2504,#2505,#369,.T.);
#3208=EDGE_CURVE('',#2505,#2505,#370,.T.);
#3209=EDGE_CURVE('',#2506,#2506,#371,.T.);
#3210=EDGE_CURVE('',#2506,#2504,#1563,.T.);
#3211=EDGE_CURVE('',#2507,#2507,#372,.T.);
#3212=EDGE_CURVE('',#2507,#2508,#1564,.T.);
#3213=EDGE_CURVE('',#2508,#2508,#373,.T.);
#3214=EDGE_CURVE('',#2509,#2509,#374,.T.);
#3215=EDGE_CURVE('',#2509,#2510,#375,.T.);
#3216=EDGE_CURVE('',#2510,#2510,#376,.T.);
#3217=EDGE_CURVE('',#2511,#2511,#377,.T.);
#3218=EDGE_CURVE('',#2511,#2509,#1565,.T.);
#3219=EDGE_CURVE('',#2512,#2512,#378,.T.);
#3220=EDGE_CURVE('',#2512,#2511,#379,.T.);
#3221=EDGE_CURVE('',#2513,#2513,#380,.T.);
#3222=EDGE_CURVE('',#2513,#2514,#381,.T.);
#3223=EDGE_CURVE('',#2514,#2514,#382,.T.);
#3224=EDGE_CURVE('',#2515,#2515,#383,.T.);
#3225=EDGE_CURVE('',#2515,#2513,#1566,.T.);
#3226=EDGE_CURVE('',#2516,#2516,#384,.T.);
#3227=EDGE_CURVE('',#2516,#2515,#385,.T.);
#3228=EDGE_CURVE('',#2517,#2517,#386,.T.);
#3229=EDGE_CURVE('',#2517,#2518,#387,.T.);
#3230=EDGE_CURVE('',#2518,#2518,#388,.T.);
#3231=EDGE_CURVE('',#2519,#2519,#389,.T.);
#3232=EDGE_CURVE('',#2519,#2517,#1567,.T.);
#3233=EDGE_CURVE('',#2520,#2520,#390,.T.);
#3234=EDGE_CURVE('',#2520,#2519,#391,.T.);
#3235=EDGE_CURVE('',#2521,#2521,#392,.T.);
#3236=EDGE_CURVE('',#2521,#2522,#393,.T.);
#3237=EDGE_CURVE('',#2522,#2522,#394,.T.);
#3238=EDGE_CURVE('',#2523,#2523,#395,.T.);
#3239=EDGE_CURVE('',#2523,#2521,#1568,.T.);
#3240=ORIENTED_EDGE('',*,*,#2524,.T.);
#3241=ORIENTED_EDGE('',*,*,#2525,.F.);
#3242=ORIENTED_EDGE('',*,*,#2526,.F.);
#3243=ORIENTED_EDGE('',*,*,#2527,.F.);
#3244=ORIENTED_EDGE('',*,*,#2528,.F.);
#3245=ORIENTED_EDGE('',*,*,#2527,.T.);
#3246=ORIENTED_EDGE('',*,*,#2529,.F.);
#3247=ORIENTED_EDGE('',*,*,#2530,.F.);
#3248=ORIENTED_EDGE('',*,*,#2531,.F.);
#3249=ORIENTED_EDGE('',*,*,#2530,.T.);
#3250=ORIENTED_EDGE('',*,*,#2532,.F.);
#3251=ORIENTED_EDGE('',*,*,#2533,.F.);
#3252=ORIENTED_EDGE('',*,*,#2525,.T.);
#3253=ORIENTED_EDGE('',*,*,#2534,.F.);
#3254=ORIENTED_EDGE('',*,*,#2535,.T.);
#3255=ORIENTED_EDGE('',*,*,#2536,.F.);
#3256=ORIENTED_EDGE('',*,*,#2533,.T.);
#3257=ORIENTED_EDGE('',*,*,#2537,.F.);
#3258=ORIENTED_EDGE('',*,*,#2538,.T.);
#3259=ORIENTED_EDGE('',*,*,#2539,.F.);
#3260=ORIENTED_EDGE('',*,*,#2540,.T.);
#3261=ORIENTED_EDGE('',*,*,#2541,.F.);
#3262=ORIENTED_EDGE('',*,*,#2542,.F.);
#3263=ORIENTED_EDGE('',*,*,#2543,.F.);
#3264=ORIENTED_EDGE('',*,*,#2544,.F.);
#3265=ORIENTED_EDGE('',*,*,#2543,.T.);
#3266=ORIENTED_EDGE('',*,*,#2545,.F.);
#3267=ORIENTED_EDGE('',*,*,#2546,.F.);
#3268=ORIENTED_EDGE('',*,*,#2547,.F.);
#3269=ORIENTED_EDGE('',*,*,#2546,.T.);
#3270=ORIENTED_EDGE('',*,*,#2548,.F.);
#3271=ORIENTED_EDGE('',*,*,#2549,.F.);
#3272=ORIENTED_EDGE('',*,*,#2541,.T.);
#3273=ORIENTED_EDGE('',*,*,#2550,.F.);
#3274=ORIENTED_EDGE('',*,*,#2551,.T.);
#3275=ORIENTED_EDGE('',*,*,#2552,.F.);
#3276=ORIENTED_EDGE('',*,*,#2549,.T.);
#3277=ORIENTED_EDGE('',*,*,#2553,.F.);
#3278=ORIENTED_EDGE('',*,*,#2554,.T.);
#3279=ORIENTED_EDGE('',*,*,#2555,.F.);
#3280=ORIENTED_EDGE('',*,*,#2556,.T.);
#3281=ORIENTED_EDGE('',*,*,#2538,.F.);
#3282=ORIENTED_EDGE('',*,*,#2557,.F.);
#3283=ORIENTED_EDGE('',*,*,#2558,.F.);
#3284=ORIENTED_EDGE('',*,*,#2559,.F.);
#3285=ORIENTED_EDGE('',*,*,#2558,.T.);
#3286=ORIENTED_EDGE('',*,*,#2560,.F.);
#3287=ORIENTED_EDGE('',*,*,#2561,.F.);
#3288=ORIENTED_EDGE('',*,*,#2562,.F.);
#3289=ORIENTED_EDGE('',*,*,#2561,.T.);
#3290=ORIENTED_EDGE('',*,*,#2563,.F.);
#3291=ORIENTED_EDGE('',*,*,#2564,.F.);
#3292=ORIENTED_EDGE('',*,*,#2564,.T.);
#3293=ORIENTED_EDGE('',*,*,#2565,.F.);
#3294=ORIENTED_EDGE('',*,*,#2566,.T.);
#3295=ORIENTED_EDGE('',*,*,#2567,.F.);
#3296=ORIENTED_EDGE('',*,*,#2568,.T.);
#3297=ORIENTED_EDGE('',*,*,#2569,.F.);
#3298=ORIENTED_EDGE('',*,*,#2570,.F.);
#3299=ORIENTED_EDGE('',*,*,#2571,.F.);
#3300=ORIENTED_EDGE('',*,*,#2572,.F.);
#3301=ORIENTED_EDGE('',*,*,#2571,.T.);
#3302=ORIENTED_EDGE('',*,*,#2573,.F.);
#3303=ORIENTED_EDGE('',*,*,#2574,.F.);
#3304=ORIENTED_EDGE('',*,*,#2575,.F.);
#3305=ORIENTED_EDGE('',*,*,#2574,.T.);
#3306=ORIENTED_EDGE('',*,*,#2576,.F.);
#3307=ORIENTED_EDGE('',*,*,#2577,.F.);
#3308=ORIENTED_EDGE('',*,*,#2569,.T.);
#3309=ORIENTED_EDGE('',*,*,#2578,.F.);
#3310=ORIENTED_EDGE('',*,*,#2579,.T.);
#3311=ORIENTED_EDGE('',*,*,#2580,.F.);
#3312=ORIENTED_EDGE('',*,*,#2577,.T.);
#3313=ORIENTED_EDGE('',*,*,#2581,.F.);
#3314=ORIENTED_EDGE('',*,*,#2582,.T.);
#3315=ORIENTED_EDGE('',*,*,#2583,.F.);
#3316=ORIENTED_EDGE('',*,*,#2584,.T.);
#3317=ORIENTED_EDGE('',*,*,#2566,.F.);
#3318=ORIENTED_EDGE('',*,*,#2585,.F.);
#3319=ORIENTED_EDGE('',*,*,#2586,.F.);
#3320=ORIENTED_EDGE('',*,*,#2587,.F.);
#3321=ORIENTED_EDGE('',*,*,#2586,.T.);
#3322=ORIENTED_EDGE('',*,*,#2588,.F.);
#3323=ORIENTED_EDGE('',*,*,#2589,.F.);
#3324=ORIENTED_EDGE('',*,*,#2590,.F.);
#3325=ORIENTED_EDGE('',*,*,#2589,.T.);
#3326=ORIENTED_EDGE('',*,*,#2591,.F.);
#3327=ORIENTED_EDGE('',*,*,#2551,.F.);
#3328=ORIENTED_EDGE('',*,*,#2592,.T.);
#3329=ORIENTED_EDGE('',*,*,#2554,.F.);
#3330=ORIENTED_EDGE('',*,*,#2593,.F.);
#3331=ORIENTED_EDGE('',*,*,#2594,.F.);
#3332=ORIENTED_EDGE('',*,*,#2595,.F.);
#3333=ORIENTED_EDGE('',*,*,#2594,.T.);
#3334=ORIENTED_EDGE('',*,*,#2596,.F.);
#3335=ORIENTED_EDGE('',*,*,#2597,.F.);
#3336=ORIENTED_EDGE('',*,*,#2598,.F.);
#3337=ORIENTED_EDGE('',*,*,#2597,.T.);
#3338=ORIENTED_EDGE('',*,*,#2599,.F.);
#3339=ORIENTED_EDGE('',*,*,#2600,.F.);
#3340=ORIENTED_EDGE('',*,*,#2600,.T.);
#3341=ORIENTED_EDGE('',*,*,#2601,.F.);
#3342=ORIENTED_EDGE('',*,*,#2602,.T.);
#3343=ORIENTED_EDGE('',*,*,#2603,.F.);
#3344=ORIENTED_EDGE('',*,*,#2604,.T.);
#3345=ORIENTED_EDGE('',*,*,#2605,.F.);
#3346=ORIENTED_EDGE('',*,*,#2606,.F.);
#3347=ORIENTED_EDGE('',*,*,#2607,.F.);
#3348=ORIENTED_EDGE('',*,*,#2608,.F.);
#3349=ORIENTED_EDGE('',*,*,#2607,.T.);
#3350=ORIENTED_EDGE('',*,*,#2609,.F.);
#3351=ORIENTED_EDGE('',*,*,#2610,.F.);
#3352=ORIENTED_EDGE('',*,*,#2611,.F.);
#3353=ORIENTED_EDGE('',*,*,#2610,.T.);
#3354=ORIENTED_EDGE('',*,*,#2612,.F.);
#3355=ORIENTED_EDGE('',*,*,#2535,.F.);
#3356=ORIENTED_EDGE('',*,*,#2605,.T.);
#3357=ORIENTED_EDGE('',*,*,#2613,.F.);
#3358=ORIENTED_EDGE('',*,*,#2614,.T.);
#3359=ORIENTED_EDGE('',*,*,#2615,.F.);
#3360=ORIENTED_EDGE('',*,*,#2616,.T.);
#3361=ORIENTED_EDGE('',*,*,#2602,.F.);
#3362=ORIENTED_EDGE('',*,*,#2617,.F.);
#3363=ORIENTED_EDGE('',*,*,#2618,.F.);
#3364=ORIENTED_EDGE('',*,*,#2619,.F.);
#3365=ORIENTED_EDGE('',*,*,#2618,.T.);
#3366=ORIENTED_EDGE('',*,*,#2620,.F.);
#3367=ORIENTED_EDGE('',*,*,#2621,.F.);
#3368=ORIENTED_EDGE('',*,*,#2622,.F.);
#3369=ORIENTED_EDGE('',*,*,#2621,.T.);
#3370=ORIENTED_EDGE('',*,*,#2623,.F.);
#3371=ORIENTED_EDGE('',*,*,#2579,.F.);
#3372=ORIENTED_EDGE('',*,*,#2624,.F.);
#3373=ORIENTED_EDGE('',*,*,#2625,.F.);
#3374=ORIENTED_EDGE('',*,*,#2626,.F.);
#3375=ORIENTED_EDGE('',*,*,#2627,.F.);
#3376=ORIENTED_EDGE('',*,*,#2628,.F.);
#3377=ORIENTED_EDGE('',*,*,#2629,.F.);
#3378=ORIENTED_EDGE('',*,*,#2630,.F.);
#3379=ORIENTED_EDGE('',*,*,#2631,.F.);
#3380=ORIENTED_EDGE('',*,*,#2625,.T.);
#3381=ORIENTED_EDGE('',*,*,#2632,.F.);
#3382=ORIENTED_EDGE('',*,*,#2633,.T.);
#3383=ORIENTED_EDGE('',*,*,#2634,.F.);
#3384=ORIENTED_EDGE('',*,*,#2631,.T.);
#3385=ORIENTED_EDGE('',*,*,#2635,.F.);
#3386=ORIENTED_EDGE('',*,*,#2636,.T.);
#3387=ORIENTED_EDGE('',*,*,#2637,.F.);
#3388=ORIENTED_EDGE('',*,*,#2627,.T.);
#3389=ORIENTED_EDGE('',*,*,#2638,.F.);
#3390=ORIENTED_EDGE('',*,*,#2639,.T.);
#3391=ORIENTED_EDGE('',*,*,#2640,.F.);
#3392=ORIENTED_EDGE('',*,*,#2629,.T.);
#3393=ORIENTED_EDGE('',*,*,#2641,.F.);
#3394=ORIENTED_EDGE('',*,*,#2642,.T.);
#3395=ORIENTED_EDGE('',*,*,#2643,.F.);
#3396=ORIENTED_EDGE('',*,*,#2644,.F.);
#3397=ORIENTED_EDGE('',*,*,#2636,.F.);
#3398=ORIENTED_EDGE('',*,*,#2645,.F.);
#3399=ORIENTED_EDGE('',*,*,#2642,.F.);
#3400=ORIENTED_EDGE('',*,*,#2646,.F.);
#3401=ORIENTED_EDGE('',*,*,#2647,.F.);
#3402=ORIENTED_EDGE('',*,*,#2648,.F.);
#3403=ORIENTED_EDGE('',*,*,#2649,.F.);
#3404=ORIENTED_EDGE('',*,*,#2649,.T.);
#3405=ORIENTED_EDGE('',*,*,#2650,.F.);
#3406=ORIENTED_EDGE('',*,*,#2651,.T.);
#3407=ORIENTED_EDGE('',*,*,#2652,.F.);
#3408=ORIENTED_EDGE('',*,*,#2647,.T.);
#3409=ORIENTED_EDGE('',*,*,#2653,.F.);
#3410=ORIENTED_EDGE('',*,*,#2654,.T.);
#3411=ORIENTED_EDGE('',*,*,#2655,.F.);
#3412=ORIENTED_EDGE('',*,*,#2656,.F.);
#3413=ORIENTED_EDGE('',*,*,#2657,.F.);
#3414=ORIENTED_EDGE('',*,*,#2658,.F.);
#3415=ORIENTED_EDGE('',*,*,#2659,.F.);
#3416=ORIENTED_EDGE('',*,*,#2660,.F.);
#3417=ORIENTED_EDGE('',*,*,#2639,.F.);
#3418=ORIENTED_EDGE('',*,*,#2661,.F.);
#3419=ORIENTED_EDGE('',*,*,#2633,.F.);
#3420=ORIENTED_EDGE('',*,*,#2657,.T.);
#3421=ORIENTED_EDGE('',*,*,#2662,.F.);
#3422=ORIENTED_EDGE('',*,*,#2663,.T.);
#3423=ORIENTED_EDGE('',*,*,#2664,.F.);
#3424=ORIENTED_EDGE('',*,*,#2659,.T.);
#3425=ORIENTED_EDGE('',*,*,#2665,.F.);
#3426=ORIENTED_EDGE('',*,*,#2666,.T.);
#3427=ORIENTED_EDGE('',*,*,#2667,.F.);
#3428=ORIENTED_EDGE('',*,*,#2668,.T.);
#3429=ORIENTED_EDGE('',*,*,#2669,.F.);
#3430=ORIENTED_EDGE('',*,*,#2670,.F.);
#3431=ORIENTED_EDGE('',*,*,#2671,.F.);
#3432=ORIENTED_EDGE('',*,*,#2672,.F.);
#3433=ORIENTED_EDGE('',*,*,#2671,.T.);
#3434=ORIENTED_EDGE('',*,*,#2673,.F.);
#3435=ORIENTED_EDGE('',*,*,#2674,.F.);
#3436=ORIENTED_EDGE('',*,*,#2675,.F.);
#3437=ORIENTED_EDGE('',*,*,#2674,.T.);
#3438=ORIENTED_EDGE('',*,*,#2676,.F.);
#3439=ORIENTED_EDGE('',*,*,#2677,.F.);
#3440=ORIENTED_EDGE('',*,*,#2669,.T.);
#3441=ORIENTED_EDGE('',*,*,#2678,.F.);
#3442=ORIENTED_EDGE('',*,*,#2679,.T.);
#3443=ORIENTED_EDGE('',*,*,#2680,.F.);
#3444=ORIENTED_EDGE('',*,*,#2677,.T.);
#3445=ORIENTED_EDGE('',*,*,#2681,.F.);
#3446=ORIENTED_EDGE('',*,*,#2682,.T.);
#3447=ORIENTED_EDGE('',*,*,#2683,.F.);
#3448=ORIENTED_EDGE('',*,*,#2684,.T.);
#3449=ORIENTED_EDGE('',*,*,#2685,.F.);
#3450=ORIENTED_EDGE('',*,*,#2686,.F.);
#3451=ORIENTED_EDGE('',*,*,#2687,.F.);
#3452=ORIENTED_EDGE('',*,*,#2688,.F.);
#3453=ORIENTED_EDGE('',*,*,#2687,.T.);
#3454=ORIENTED_EDGE('',*,*,#2689,.F.);
#3455=ORIENTED_EDGE('',*,*,#2690,.F.);
#3456=ORIENTED_EDGE('',*,*,#2691,.F.);
#3457=ORIENTED_EDGE('',*,*,#2690,.T.);
#3458=ORIENTED_EDGE('',*,*,#2692,.F.);
#3459=ORIENTED_EDGE('',*,*,#2693,.F.);
#3460=ORIENTED_EDGE('',*,*,#2685,.T.);
#3461=ORIENTED_EDGE('',*,*,#2694,.F.);
#3462=ORIENTED_EDGE('',*,*,#2695,.T.);
#3463=ORIENTED_EDGE('',*,*,#2696,.F.);
#3464=ORIENTED_EDGE('',*,*,#2693,.T.);
#3465=ORIENTED_EDGE('',*,*,#2697,.F.);
#3466=ORIENTED_EDGE('',*,*,#2698,.T.);
#3467=ORIENTED_EDGE('',*,*,#2699,.F.);
#3468=ORIENTED_EDGE('',*,*,#2700,.T.);
#3469=ORIENTED_EDGE('',*,*,#2698,.F.);
#3470=ORIENTED_EDGE('',*,*,#2701,.F.);
#3471=ORIENTED_EDGE('',*,*,#2702,.F.);
#3472=ORIENTED_EDGE('',*,*,#2703,.F.);
#3473=ORIENTED_EDGE('',*,*,#2702,.T.);
#3474=ORIENTED_EDGE('',*,*,#2704,.F.);
#3475=ORIENTED_EDGE('',*,*,#2705,.F.);
#3476=ORIENTED_EDGE('',*,*,#2706,.F.);
#3477=ORIENTED_EDGE('',*,*,#2705,.T.);
#3478=ORIENTED_EDGE('',*,*,#2707,.F.);
#3479=ORIENTED_EDGE('',*,*,#2708,.F.);
#3480=ORIENTED_EDGE('',*,*,#2708,.T.);
#3481=ORIENTED_EDGE('',*,*,#2709,.F.);
#3482=ORIENTED_EDGE('',*,*,#2710,.T.);
#3483=ORIENTED_EDGE('',*,*,#2711,.F.);
#3484=ORIENTED_EDGE('',*,*,#2712,.T.);
#3485=ORIENTED_EDGE('',*,*,#2710,.F.);
#3486=ORIENTED_EDGE('',*,*,#2713,.F.);
#3487=ORIENTED_EDGE('',*,*,#2714,.F.);
#3488=ORIENTED_EDGE('',*,*,#2715,.F.);
#3489=ORIENTED_EDGE('',*,*,#2714,.T.);
#3490=ORIENTED_EDGE('',*,*,#2716,.F.);
#3491=ORIENTED_EDGE('',*,*,#2717,.F.);
#3492=ORIENTED_EDGE('',*,*,#2718,.F.);
#3493=ORIENTED_EDGE('',*,*,#2717,.T.);
#3494=ORIENTED_EDGE('',*,*,#2719,.F.);
#3495=ORIENTED_EDGE('',*,*,#2679,.F.);
#3496=ORIENTED_EDGE('',*,*,#2720,.T.);
#3497=ORIENTED_EDGE('',*,*,#2682,.F.);
#3498=ORIENTED_EDGE('',*,*,#2721,.F.);
#3499=ORIENTED_EDGE('',*,*,#2722,.F.);
#3500=ORIENTED_EDGE('',*,*,#2723,.F.);
#3501=ORIENTED_EDGE('',*,*,#2722,.T.);
#3502=ORIENTED_EDGE('',*,*,#2724,.F.);
#3503=ORIENTED_EDGE('',*,*,#2725,.F.);
#3504=ORIENTED_EDGE('',*,*,#2726,.F.);
#3505=ORIENTED_EDGE('',*,*,#2725,.T.);
#3506=ORIENTED_EDGE('',*,*,#2727,.F.);
#3507=ORIENTED_EDGE('',*,*,#2728,.F.);
#3508=ORIENTED_EDGE('',*,*,#2728,.T.);
#3509=ORIENTED_EDGE('',*,*,#2729,.F.);
#3510=ORIENTED_EDGE('',*,*,#2730,.T.);
#3511=ORIENTED_EDGE('',*,*,#2731,.F.);
#3512=ORIENTED_EDGE('',*,*,#2732,.T.);
#3513=ORIENTED_EDGE('',*,*,#2730,.F.);
#3514=ORIENTED_EDGE('',*,*,#2733,.F.);
#3515=ORIENTED_EDGE('',*,*,#2734,.F.);
#3516=ORIENTED_EDGE('',*,*,#2735,.F.);
#3517=ORIENTED_EDGE('',*,*,#2734,.T.);
#3518=ORIENTED_EDGE('',*,*,#2736,.F.);
#3519=ORIENTED_EDGE('',*,*,#2737,.F.);
#3520=ORIENTED_EDGE('',*,*,#2738,.F.);
#3521=ORIENTED_EDGE('',*,*,#2737,.T.);
#3522=ORIENTED_EDGE('',*,*,#2739,.F.);
#3523=ORIENTED_EDGE('',*,*,#2614,.F.);
#3524=ORIENTED_EDGE('',*,*,#2740,.F.);
#3525=ORIENTED_EDGE('',*,*,#2741,.F.);
#3526=ORIENTED_EDGE('',*,*,#2742,.F.);
#3527=ORIENTED_EDGE('',*,*,#2743,.F.);
#3528=ORIENTED_EDGE('',*,*,#2744,.F.);
#3529=ORIENTED_EDGE('',*,*,#2745,.F.);
#3530=ORIENTED_EDGE('',*,*,#2746,.F.);
#3531=ORIENTED_EDGE('',*,*,#2747,.F.);
#3532=ORIENTED_EDGE('',*,*,#2741,.T.);
#3533=ORIENTED_EDGE('',*,*,#2748,.F.);
#3534=ORIENTED_EDGE('',*,*,#2749,.T.);
#3535=ORIENTED_EDGE('',*,*,#2750,.F.);
#3536=ORIENTED_EDGE('',*,*,#2747,.T.);
#3537=ORIENTED_EDGE('',*,*,#2751,.F.);
#3538=ORIENTED_EDGE('',*,*,#2752,.T.);
#3539=ORIENTED_EDGE('',*,*,#2753,.F.);
#3540=ORIENTED_EDGE('',*,*,#2743,.T.);
#3541=ORIENTED_EDGE('',*,*,#2754,.F.);
#3542=ORIENTED_EDGE('',*,*,#2755,.T.);
#3543=ORIENTED_EDGE('',*,*,#2756,.F.);
#3544=ORIENTED_EDGE('',*,*,#2745,.T.);
#3545=ORIENTED_EDGE('',*,*,#2757,.F.);
#3546=ORIENTED_EDGE('',*,*,#2758,.T.);
#3547=ORIENTED_EDGE('',*,*,#2759,.F.);
#3548=ORIENTED_EDGE('',*,*,#2760,.F.);
#3549=ORIENTED_EDGE('',*,*,#2752,.F.);
#3550=ORIENTED_EDGE('',*,*,#2761,.F.);
#3551=ORIENTED_EDGE('',*,*,#2758,.F.);
#3552=ORIENTED_EDGE('',*,*,#2762,.F.);
#3553=ORIENTED_EDGE('',*,*,#2763,.F.);
#3554=ORIENTED_EDGE('',*,*,#2764,.F.);
#3555=ORIENTED_EDGE('',*,*,#2765,.F.);
#3556=ORIENTED_EDGE('',*,*,#2765,.T.);
#3557=ORIENTED_EDGE('',*,*,#2766,.F.);
#3558=ORIENTED_EDGE('',*,*,#2767,.T.);
#3559=ORIENTED_EDGE('',*,*,#2768,.F.);
#3560=ORIENTED_EDGE('',*,*,#2763,.T.);
#3561=ORIENTED_EDGE('',*,*,#2769,.F.);
#3562=ORIENTED_EDGE('',*,*,#2770,.T.);
#3563=ORIENTED_EDGE('',*,*,#2771,.F.);
#3564=ORIENTED_EDGE('',*,*,#2772,.F.);
#3565=ORIENTED_EDGE('',*,*,#2773,.F.);
#3566=ORIENTED_EDGE('',*,*,#2774,.F.);
#3567=ORIENTED_EDGE('',*,*,#2775,.F.);
#3568=ORIENTED_EDGE('',*,*,#2776,.F.);
#3569=ORIENTED_EDGE('',*,*,#2777,.F.);
#3570=ORIENTED_EDGE('',*,*,#2778,.F.);
#3571=ORIENTED_EDGE('',*,*,#2779,.F.);
#3572=ORIENTED_EDGE('',*,*,#2773,.T.);
#3573=ORIENTED_EDGE('',*,*,#2780,.F.);
#3574=ORIENTED_EDGE('',*,*,#2781,.T.);
#3575=ORIENTED_EDGE('',*,*,#2782,.F.);
#3576=ORIENTED_EDGE('',*,*,#2779,.T.);
#3577=ORIENTED_EDGE('',*,*,#2783,.F.);
#3578=ORIENTED_EDGE('',*,*,#2784,.T.);
#3579=ORIENTED_EDGE('',*,*,#2785,.F.);
#3580=ORIENTED_EDGE('',*,*,#2775,.T.);
#3581=ORIENTED_EDGE('',*,*,#2786,.F.);
#3582=ORIENTED_EDGE('',*,*,#2787,.T.);
#3583=ORIENTED_EDGE('',*,*,#2788,.F.);
#3584=ORIENTED_EDGE('',*,*,#2777,.T.);
#3585=ORIENTED_EDGE('',*,*,#2789,.F.);
#3586=ORIENTED_EDGE('',*,*,#2790,.T.);
#3587=ORIENTED_EDGE('',*,*,#2791,.F.);
#3588=ORIENTED_EDGE('',*,*,#2792,.F.);
#3589=ORIENTED_EDGE('',*,*,#2793,.F.);
#3590=ORIENTED_EDGE('',*,*,#2794,.F.);
#3591=ORIENTED_EDGE('',*,*,#2795,.F.);
#3592=ORIENTED_EDGE('',*,*,#2796,.F.);
#3593=ORIENTED_EDGE('',*,*,#2797,.F.);
#3594=ORIENTED_EDGE('',*,*,#2798,.F.);
#3595=ORIENTED_EDGE('',*,*,#2799,.F.);
#3596=ORIENTED_EDGE('',*,*,#2793,.T.);
#3597=ORIENTED_EDGE('',*,*,#2800,.F.);
#3598=ORIENTED_EDGE('',*,*,#2801,.T.);
#3599=ORIENTED_EDGE('',*,*,#2802,.F.);
#3600=ORIENTED_EDGE('',*,*,#2799,.T.);
#3601=ORIENTED_EDGE('',*,*,#2803,.F.);
#3602=ORIENTED_EDGE('',*,*,#2804,.T.);
#3603=ORIENTED_EDGE('',*,*,#2805,.F.);
#3604=ORIENTED_EDGE('',*,*,#2795,.T.);
#3605=ORIENTED_EDGE('',*,*,#2806,.F.);
#3606=ORIENTED_EDGE('',*,*,#2807,.T.);
#3607=ORIENTED_EDGE('',*,*,#2808,.F.);
#3608=ORIENTED_EDGE('',*,*,#2797,.T.);
#3609=ORIENTED_EDGE('',*,*,#2809,.F.);
#3610=ORIENTED_EDGE('',*,*,#2810,.T.);
#3611=ORIENTED_EDGE('',*,*,#2811,.F.);
#3612=ORIENTED_EDGE('',*,*,#2812,.F.);
#3613=ORIENTED_EDGE('',*,*,#2767,.F.);
#3614=ORIENTED_EDGE('',*,*,#2813,.F.);
#3615=ORIENTED_EDGE('',*,*,#2770,.F.);
#3616=ORIENTED_EDGE('',*,*,#2814,.F.);
#3617=ORIENTED_EDGE('',*,*,#2815,.F.);
#3618=ORIENTED_EDGE('',*,*,#2816,.F.);
#3619=ORIENTED_EDGE('',*,*,#2817,.F.);
#3620=ORIENTED_EDGE('',*,*,#2817,.T.);
#3621=ORIENTED_EDGE('',*,*,#2818,.F.);
#3622=ORIENTED_EDGE('',*,*,#2819,.T.);
#3623=ORIENTED_EDGE('',*,*,#2820,.F.);
#3624=ORIENTED_EDGE('',*,*,#2815,.T.);
#3625=ORIENTED_EDGE('',*,*,#2821,.F.);
#3626=ORIENTED_EDGE('',*,*,#2822,.T.);
#3627=ORIENTED_EDGE('',*,*,#2823,.F.);
#3628=ORIENTED_EDGE('',*,*,#2824,.F.);
#3629=ORIENTED_EDGE('',*,*,#2804,.F.);
#3630=ORIENTED_EDGE('',*,*,#2825,.F.);
#3631=ORIENTED_EDGE('',*,*,#2810,.F.);
#3632=ORIENTED_EDGE('',*,*,#2826,.F.);
#3633=ORIENTED_EDGE('',*,*,#2787,.F.);
#3634=ORIENTED_EDGE('',*,*,#2827,.F.);
#3635=ORIENTED_EDGE('',*,*,#2781,.F.);
#3636=ORIENTED_EDGE('',*,*,#2828,.F.);
#3637=ORIENTED_EDGE('',*,*,#2819,.F.);
#3638=ORIENTED_EDGE('',*,*,#2829,.F.);
#3639=ORIENTED_EDGE('',*,*,#2822,.F.);
#3640=ORIENTED_EDGE('',*,*,#2830,.F.);
#3641=ORIENTED_EDGE('',*,*,#2831,.F.);
#3642=ORIENTED_EDGE('',*,*,#2832,.F.);
#3643=ORIENTED_EDGE('',*,*,#2833,.F.);
#3644=ORIENTED_EDGE('',*,*,#2833,.T.);
#3645=ORIENTED_EDGE('',*,*,#2834,.F.);
#3646=ORIENTED_EDGE('',*,*,#2835,.T.);
#3647=ORIENTED_EDGE('',*,*,#2836,.F.);
#3648=ORIENTED_EDGE('',*,*,#2831,.T.);
#3649=ORIENTED_EDGE('',*,*,#2837,.F.);
#3650=ORIENTED_EDGE('',*,*,#2838,.T.);
#3651=ORIENTED_EDGE('',*,*,#2839,.F.);
#3652=ORIENTED_EDGE('',*,*,#2840,.F.);
#3653=ORIENTED_EDGE('',*,*,#2784,.F.);
#3654=ORIENTED_EDGE('',*,*,#2841,.F.);
#3655=ORIENTED_EDGE('',*,*,#2790,.F.);
#3656=ORIENTED_EDGE('',*,*,#2842,.F.);
#3657=ORIENTED_EDGE('',*,*,#2755,.F.);
#3658=ORIENTED_EDGE('',*,*,#2843,.F.);
#3659=ORIENTED_EDGE('',*,*,#2749,.F.);
#3660=ORIENTED_EDGE('',*,*,#2844,.T.);
#3661=ORIENTED_EDGE('',*,*,#2845,.F.);
#3662=ORIENTED_EDGE('',*,*,#2846,.F.);
#3663=ORIENTED_EDGE('',*,*,#2847,.F.);
#3664=ORIENTED_EDGE('',*,*,#2848,.F.);
#3665=ORIENTED_EDGE('',*,*,#2847,.T.);
#3666=ORIENTED_EDGE('',*,*,#2849,.F.);
#3667=ORIENTED_EDGE('',*,*,#2850,.F.);
#3668=ORIENTED_EDGE('',*,*,#2851,.F.);
#3669=ORIENTED_EDGE('',*,*,#2850,.T.);
#3670=ORIENTED_EDGE('',*,*,#2852,.F.);
#3671=ORIENTED_EDGE('',*,*,#2853,.F.);
#3672=ORIENTED_EDGE('',*,*,#2845,.T.);
#3673=ORIENTED_EDGE('',*,*,#2854,.F.);
#3674=ORIENTED_EDGE('',*,*,#2855,.T.);
#3675=ORIENTED_EDGE('',*,*,#2856,.F.);
#3676=ORIENTED_EDGE('',*,*,#2853,.T.);
#3677=ORIENTED_EDGE('',*,*,#2857,.F.);
#3678=ORIENTED_EDGE('',*,*,#2858,.T.);
#3679=ORIENTED_EDGE('',*,*,#2859,.F.);
#3680=ORIENTED_EDGE('',*,*,#2860,.T.);
#3681=ORIENTED_EDGE('',*,*,#2858,.F.);
#3682=ORIENTED_EDGE('',*,*,#2861,.F.);
#3683=ORIENTED_EDGE('',*,*,#2862,.F.);
#3684=ORIENTED_EDGE('',*,*,#2863,.F.);
#3685=ORIENTED_EDGE('',*,*,#2862,.T.);
#3686=ORIENTED_EDGE('',*,*,#2864,.F.);
#3687=ORIENTED_EDGE('',*,*,#2865,.F.);
#3688=ORIENTED_EDGE('',*,*,#2866,.F.);
#3689=ORIENTED_EDGE('',*,*,#2865,.T.);
#3690=ORIENTED_EDGE('',*,*,#2867,.F.);
#3691=ORIENTED_EDGE('',*,*,#2868,.F.);
#3692=ORIENTED_EDGE('',*,*,#2868,.T.);
#3693=ORIENTED_EDGE('',*,*,#2869,.F.);
#3694=ORIENTED_EDGE('',*,*,#2870,.T.);
#3695=ORIENTED_EDGE('',*,*,#2871,.F.);
#3696=ORIENTED_EDGE('',*,*,#2872,.T.);
#3697=ORIENTED_EDGE('',*,*,#2873,.F.);
#3698=ORIENTED_EDGE('',*,*,#2874,.F.);
#3699=ORIENTED_EDGE('',*,*,#2875,.F.);
#3700=ORIENTED_EDGE('',*,*,#2876,.F.);
#3701=ORIENTED_EDGE('',*,*,#2875,.T.);
#3702=ORIENTED_EDGE('',*,*,#2877,.F.);
#3703=ORIENTED_EDGE('',*,*,#2878,.F.);
#3704=ORIENTED_EDGE('',*,*,#2879,.F.);
#3705=ORIENTED_EDGE('',*,*,#2878,.T.);
#3706=ORIENTED_EDGE('',*,*,#2880,.F.);
#3707=ORIENTED_EDGE('',*,*,#2881,.F.);
#3708=ORIENTED_EDGE('',*,*,#2873,.T.);
#3709=ORIENTED_EDGE('',*,*,#2882,.F.);
#3710=ORIENTED_EDGE('',*,*,#2883,.T.);
#3711=ORIENTED_EDGE('',*,*,#2884,.F.);
#3712=ORIENTED_EDGE('',*,*,#2881,.T.);
#3713=ORIENTED_EDGE('',*,*,#2885,.F.);
#3714=ORIENTED_EDGE('',*,*,#2886,.T.);
#3715=ORIENTED_EDGE('',*,*,#2887,.F.);
#3716=ORIENTED_EDGE('',*,*,#2888,.T.);
#3717=ORIENTED_EDGE('',*,*,#2889,.F.);
#3718=ORIENTED_EDGE('',*,*,#2890,.F.);
#3719=ORIENTED_EDGE('',*,*,#2891,.F.);
#3720=ORIENTED_EDGE('',*,*,#2892,.F.);
#3721=ORIENTED_EDGE('',*,*,#2891,.T.);
#3722=ORIENTED_EDGE('',*,*,#2893,.F.);
#3723=ORIENTED_EDGE('',*,*,#2894,.F.);
#3724=ORIENTED_EDGE('',*,*,#2895,.F.);
#3725=ORIENTED_EDGE('',*,*,#2894,.T.);
#3726=ORIENTED_EDGE('',*,*,#2896,.F.);
#3727=ORIENTED_EDGE('',*,*,#2897,.F.);
#3728=ORIENTED_EDGE('',*,*,#2889,.T.);
#3729=ORIENTED_EDGE('',*,*,#2898,.F.);
#3730=ORIENTED_EDGE('',*,*,#2899,.T.);
#3731=ORIENTED_EDGE('',*,*,#2900,.F.);
#3732=ORIENTED_EDGE('',*,*,#2897,.T.);
#3733=ORIENTED_EDGE('',*,*,#2901,.F.);
#3734=ORIENTED_EDGE('',*,*,#2902,.T.);
#3735=ORIENTED_EDGE('',*,*,#2903,.F.);
#3736=ORIENTED_EDGE('',*,*,#2904,.T.);
#3737=ORIENTED_EDGE('',*,*,#2886,.F.);
#3738=ORIENTED_EDGE('',*,*,#2905,.F.);
#3739=ORIENTED_EDGE('',*,*,#2906,.F.);
#3740=ORIENTED_EDGE('',*,*,#2907,.F.);
#3741=ORIENTED_EDGE('',*,*,#2906,.T.);
#3742=ORIENTED_EDGE('',*,*,#2908,.F.);
#3743=ORIENTED_EDGE('',*,*,#2909,.F.);
#3744=ORIENTED_EDGE('',*,*,#2910,.F.);
#3745=ORIENTED_EDGE('',*,*,#2909,.T.);
#3746=ORIENTED_EDGE('',*,*,#2911,.F.);
#3747=ORIENTED_EDGE('',*,*,#2899,.F.);
#3748=ORIENTED_EDGE('',*,*,#2912,.T.);
#3749=ORIENTED_EDGE('',*,*,#2582,.F.);
#3750=ORIENTED_EDGE('',*,*,#2913,.F.);
#3751=ORIENTED_EDGE('',*,*,#2914,.F.);
#3752=ORIENTED_EDGE('',*,*,#2915,.F.);
#3753=ORIENTED_EDGE('',*,*,#2914,.T.);
#3754=ORIENTED_EDGE('',*,*,#2916,.F.);
#3755=ORIENTED_EDGE('',*,*,#2917,.F.);
#3756=ORIENTED_EDGE('',*,*,#2918,.F.);
#3757=ORIENTED_EDGE('',*,*,#2917,.T.);
#3758=ORIENTED_EDGE('',*,*,#2919,.F.);
#3759=ORIENTED_EDGE('',*,*,#2855,.F.);
#3760=ORIENTED_EDGE('',*,*,#2920,.T.);
#3761=ORIENTED_EDGE('',*,*,#2870,.F.);
#3762=ORIENTED_EDGE('',*,*,#2921,.F.);
#3763=ORIENTED_EDGE('',*,*,#2922,.F.);
#3764=ORIENTED_EDGE('',*,*,#2923,.F.);
#3765=ORIENTED_EDGE('',*,*,#2922,.T.);
#3766=ORIENTED_EDGE('',*,*,#2924,.F.);
#3767=ORIENTED_EDGE('',*,*,#2925,.F.);
#3768=ORIENTED_EDGE('',*,*,#2926,.F.);
#3769=ORIENTED_EDGE('',*,*,#2925,.T.);
#3770=ORIENTED_EDGE('',*,*,#2927,.F.);
#3771=ORIENTED_EDGE('',*,*,#2883,.F.);
#3772=ORIENTED_EDGE('',*,*,#2928,.T.);
#3773=ORIENTED_EDGE('',*,*,#2902,.F.);
#3774=ORIENTED_EDGE('',*,*,#2929,.F.);
#3775=ORIENTED_EDGE('',*,*,#2930,.F.);
#3776=ORIENTED_EDGE('',*,*,#2931,.F.);
#3777=ORIENTED_EDGE('',*,*,#2930,.T.);
#3778=ORIENTED_EDGE('',*,*,#2932,.F.);
#3779=ORIENTED_EDGE('',*,*,#2933,.F.);
#3780=ORIENTED_EDGE('',*,*,#2934,.F.);
#3781=ORIENTED_EDGE('',*,*,#2933,.T.);
#3782=ORIENTED_EDGE('',*,*,#2935,.F.);
#3783=ORIENTED_EDGE('',*,*,#2936,.F.);
#3784=ORIENTED_EDGE('',*,*,#2936,.T.);
#3785=ORIENTED_EDGE('',*,*,#2937,.F.);
#3786=ORIENTED_EDGE('',*,*,#2938,.T.);
#3787=ORIENTED_EDGE('',*,*,#2939,.F.);
#3788=ORIENTED_EDGE('',*,*,#2940,.F.);
#3789=ORIENTED_EDGE('',*,*,#2835,.F.);
#3790=ORIENTED_EDGE('',*,*,#2941,.F.);
#3791=ORIENTED_EDGE('',*,*,#2838,.F.);
#3792=ORIENTED_EDGE('',*,*,#2942,.F.);
#3793=ORIENTED_EDGE('',*,*,#2943,.F.);
#3794=ORIENTED_EDGE('',*,*,#2944,.F.);
#3795=ORIENTED_EDGE('',*,*,#2945,.F.);
#3796=ORIENTED_EDGE('',*,*,#2945,.T.);
#3797=ORIENTED_EDGE('',*,*,#2946,.F.);
#3798=ORIENTED_EDGE('',*,*,#2947,.T.);
#3799=ORIENTED_EDGE('',*,*,#2948,.F.);
#3800=ORIENTED_EDGE('',*,*,#2943,.T.);
#3801=ORIENTED_EDGE('',*,*,#2949,.F.);
#3802=ORIENTED_EDGE('',*,*,#2950,.T.);
#3803=ORIENTED_EDGE('',*,*,#2951,.F.);
#3804=ORIENTED_EDGE('',*,*,#2952,.F.);
#3805=ORIENTED_EDGE('',*,*,#2953,.F.);
#3806=ORIENTED_EDGE('',*,*,#2954,.F.);
#3807=ORIENTED_EDGE('',*,*,#2955,.F.);
#3808=ORIENTED_EDGE('',*,*,#2956,.F.);
#3809=ORIENTED_EDGE('',*,*,#2666,.F.);
#3810=ORIENTED_EDGE('',*,*,#2957,.F.);
#3811=ORIENTED_EDGE('',*,*,#2663,.F.);
#3812=ORIENTED_EDGE('',*,*,#2953,.T.);
#3813=ORIENTED_EDGE('',*,*,#2958,.F.);
#3814=ORIENTED_EDGE('',*,*,#2959,.T.);
#3815=ORIENTED_EDGE('',*,*,#2960,.F.);
#3816=ORIENTED_EDGE('',*,*,#2955,.T.);
#3817=ORIENTED_EDGE('',*,*,#2961,.F.);
#3818=ORIENTED_EDGE('',*,*,#2962,.T.);
#3819=ORIENTED_EDGE('',*,*,#2963,.F.);
#3820=ORIENTED_EDGE('',*,*,#2964,.F.);
#3821=ORIENTED_EDGE('',*,*,#2947,.F.);
#3822=ORIENTED_EDGE('',*,*,#2965,.F.);
#3823=ORIENTED_EDGE('',*,*,#2950,.F.);
#3824=ORIENTED_EDGE('',*,*,#2966,.F.);
#3825=ORIENTED_EDGE('',*,*,#2962,.F.);
#3826=ORIENTED_EDGE('',*,*,#2967,.F.);
#3827=ORIENTED_EDGE('',*,*,#2959,.F.);
#3828=ORIENTED_EDGE('',*,*,#2968,.T.);
#3829=ORIENTED_EDGE('',*,*,#2969,.F.);
#3830=ORIENTED_EDGE('',*,*,#2970,.F.);
#3831=ORIENTED_EDGE('',*,*,#2971,.F.);
#3832=ORIENTED_EDGE('',*,*,#2972,.F.);
#3833=ORIENTED_EDGE('',*,*,#2971,.T.);
#3834=ORIENTED_EDGE('',*,*,#2973,.F.);
#3835=ORIENTED_EDGE('',*,*,#2974,.F.);
#3836=ORIENTED_EDGE('',*,*,#2975,.F.);
#3837=ORIENTED_EDGE('',*,*,#2974,.T.);
#3838=ORIENTED_EDGE('',*,*,#2976,.F.);
#3839=ORIENTED_EDGE('',*,*,#2977,.F.);
#3840=ORIENTED_EDGE('',*,*,#2969,.T.);
#3841=ORIENTED_EDGE('',*,*,#2978,.F.);
#3842=ORIENTED_EDGE('',*,*,#2979,.T.);
#3843=ORIENTED_EDGE('',*,*,#2980,.F.);
#3844=ORIENTED_EDGE('',*,*,#2977,.T.);
#3845=ORIENTED_EDGE('',*,*,#2981,.F.);
#3846=ORIENTED_EDGE('',*,*,#2982,.T.);
#3847=ORIENTED_EDGE('',*,*,#2983,.F.);
#3848=ORIENTED_EDGE('',*,*,#2984,.T.);
#3849=ORIENTED_EDGE('',*,*,#2982,.F.);
#3850=ORIENTED_EDGE('',*,*,#2985,.F.);
#3851=ORIENTED_EDGE('',*,*,#2986,.F.);
#3852=ORIENTED_EDGE('',*,*,#2987,.F.);
#3853=ORIENTED_EDGE('',*,*,#2986,.T.);
#3854=ORIENTED_EDGE('',*,*,#2988,.F.);
#3855=ORIENTED_EDGE('',*,*,#2989,.F.);
#3856=ORIENTED_EDGE('',*,*,#2990,.F.);
#3857=ORIENTED_EDGE('',*,*,#2989,.T.);
#3858=ORIENTED_EDGE('',*,*,#2991,.F.);
#3859=ORIENTED_EDGE('',*,*,#2992,.F.);
#3860=ORIENTED_EDGE('',*,*,#2992,.T.);
#3861=ORIENTED_EDGE('',*,*,#2993,.F.);
#3862=ORIENTED_EDGE('',*,*,#2994,.T.);
#3863=ORIENTED_EDGE('',*,*,#2995,.F.);
#3864=ORIENTED_EDGE('',*,*,#2996,.T.);
#3865=ORIENTED_EDGE('',*,*,#2997,.F.);
#3866=ORIENTED_EDGE('',*,*,#2998,.F.);
#3867=ORIENTED_EDGE('',*,*,#2999,.F.);
#3868=ORIENTED_EDGE('',*,*,#3000,.F.);
#3869=ORIENTED_EDGE('',*,*,#2999,.T.);
#3870=ORIENTED_EDGE('',*,*,#3001,.F.);
#3871=ORIENTED_EDGE('',*,*,#3002,.F.);
#3872=ORIENTED_EDGE('',*,*,#3003,.F.);
#3873=ORIENTED_EDGE('',*,*,#3002,.T.);
#3874=ORIENTED_EDGE('',*,*,#3004,.F.);
#3875=ORIENTED_EDGE('',*,*,#3005,.F.);
#3876=ORIENTED_EDGE('',*,*,#2997,.T.);
#3877=ORIENTED_EDGE('',*,*,#3006,.F.);
#3878=ORIENTED_EDGE('',*,*,#3007,.T.);
#3879=ORIENTED_EDGE('',*,*,#3008,.F.);
#3880=ORIENTED_EDGE('',*,*,#3005,.T.);
#3881=ORIENTED_EDGE('',*,*,#3009,.F.);
#3882=ORIENTED_EDGE('',*,*,#3010,.T.);
#3883=ORIENTED_EDGE('',*,*,#3011,.F.);
#3884=ORIENTED_EDGE('',*,*,#3012,.T.);
#3885=ORIENTED_EDGE('',*,*,#2994,.F.);
#3886=ORIENTED_EDGE('',*,*,#3013,.F.);
#3887=ORIENTED_EDGE('',*,*,#3014,.F.);
#3888=ORIENTED_EDGE('',*,*,#3015,.F.);
#3889=ORIENTED_EDGE('',*,*,#3014,.T.);
#3890=ORIENTED_EDGE('',*,*,#3016,.F.);
#3891=ORIENTED_EDGE('',*,*,#3017,.F.);
#3892=ORIENTED_EDGE('',*,*,#3018,.F.);
#3893=ORIENTED_EDGE('',*,*,#3017,.T.);
#3894=ORIENTED_EDGE('',*,*,#3019,.F.);
#3895=ORIENTED_EDGE('',*,*,#3020,.F.);
#3896=ORIENTED_EDGE('',*,*,#3020,.T.);
#3897=ORIENTED_EDGE('',*,*,#3021,.F.);
#3898=ORIENTED_EDGE('',*,*,#3022,.T.);
#3899=ORIENTED_EDGE('',*,*,#3023,.F.);
#3900=ORIENTED_EDGE('',*,*,#3024,.T.);
#3901=ORIENTED_EDGE('',*,*,#2938,.F.);
#3902=ORIENTED_EDGE('',*,*,#3025,.F.);
#3903=ORIENTED_EDGE('',*,*,#3026,.F.);
#3904=ORIENTED_EDGE('',*,*,#3027,.F.);
#3905=ORIENTED_EDGE('',*,*,#3026,.T.);
#3906=ORIENTED_EDGE('',*,*,#3028,.F.);
#3907=ORIENTED_EDGE('',*,*,#3029,.F.);
#3908=ORIENTED_EDGE('',*,*,#3030,.F.);
#3909=ORIENTED_EDGE('',*,*,#3029,.T.);
#3910=ORIENTED_EDGE('',*,*,#3031,.F.);
#3911=ORIENTED_EDGE('',*,*,#3032,.F.);
#3912=ORIENTED_EDGE('',*,*,#3032,.T.);
#3913=ORIENTED_EDGE('',*,*,#3033,.F.);
#3914=ORIENTED_EDGE('',*,*,#3034,.T.);
#3915=ORIENTED_EDGE('',*,*,#3035,.F.);
#3916=ORIENTED_EDGE('',*,*,#3036,.T.);
#3917=ORIENTED_EDGE('',*,*,#3010,.F.);
#3918=ORIENTED_EDGE('',*,*,#3037,.F.);
#3919=ORIENTED_EDGE('',*,*,#3038,.F.);
#3920=ORIENTED_EDGE('',*,*,#3039,.F.);
#3921=ORIENTED_EDGE('',*,*,#3038,.T.);
#3922=ORIENTED_EDGE('',*,*,#3040,.F.);
#3923=ORIENTED_EDGE('',*,*,#3041,.F.);
#3924=ORIENTED_EDGE('',*,*,#3042,.F.);
#3925=ORIENTED_EDGE('',*,*,#3041,.T.);
#3926=ORIENTED_EDGE('',*,*,#3043,.F.);
#3927=ORIENTED_EDGE('',*,*,#2695,.F.);
#3928=ORIENTED_EDGE('',*,*,#3044,.T.);
#3929=ORIENTED_EDGE('',*,*,#3022,.F.);
#3930=ORIENTED_EDGE('',*,*,#3045,.F.);
#3931=ORIENTED_EDGE('',*,*,#3046,.F.);
#3932=ORIENTED_EDGE('',*,*,#3047,.F.);
#3933=ORIENTED_EDGE('',*,*,#3046,.T.);
#3934=ORIENTED_EDGE('',*,*,#3048,.F.);
#3935=ORIENTED_EDGE('',*,*,#3049,.F.);
#3936=ORIENTED_EDGE('',*,*,#3050,.F.);
#3937=ORIENTED_EDGE('',*,*,#3049,.T.);
#3938=ORIENTED_EDGE('',*,*,#3051,.F.);
#3939=ORIENTED_EDGE('',*,*,#3007,.F.);
#3940=ORIENTED_EDGE('',*,*,#3052,.T.);
#3941=ORIENTED_EDGE('',*,*,#3034,.F.);
#3942=ORIENTED_EDGE('',*,*,#3053,.F.);
#3943=ORIENTED_EDGE('',*,*,#3054,.F.);
#3944=ORIENTED_EDGE('',*,*,#3055,.F.);
#3945=ORIENTED_EDGE('',*,*,#3054,.T.);
#3946=ORIENTED_EDGE('',*,*,#3056,.F.);
#3947=ORIENTED_EDGE('',*,*,#3057,.F.);
#3948=ORIENTED_EDGE('',*,*,#3058,.F.);
#3949=ORIENTED_EDGE('',*,*,#3057,.T.);
#3950=ORIENTED_EDGE('',*,*,#3059,.F.);
#3951=ORIENTED_EDGE('',*,*,#2979,.F.);
#3952=ORIENTED_EDGE('',*,*,#3060,.F.);
#3953=ORIENTED_EDGE('',*,*,#2651,.F.);
#3954=ORIENTED_EDGE('',*,*,#3061,.F.);
#3955=ORIENTED_EDGE('',*,*,#2654,.F.);
#3956=ORIENTED_EDGE('',*,*,#3062,.F.);
#3957=ORIENTED_EDGE('',*,*,#2807,.F.);
#3958=ORIENTED_EDGE('',*,*,#3063,.F.);
#3959=ORIENTED_EDGE('',*,*,#2801,.F.);
#3960=ORIENTED_EDGE('',*,*,#3064,.F.);
#3961=ORIENTED_EDGE('',*,*,#3065,.T.);
#3962=ORIENTED_EDGE('',*,*,#3066,.F.);
#3963=ORIENTED_EDGE('',*,*,#3065,.F.);
#3964=ORIENTED_EDGE('',*,*,#2978,.T.);
#3965=ORIENTED_EDGE('',*,*,#2968,.F.);
#3966=ORIENTED_EDGE('',*,*,#2972,.T.);
#3967=ORIENTED_EDGE('',*,*,#2975,.T.);
#3968=ORIENTED_EDGE('',*,*,#2983,.T.);
#3969=ORIENTED_EDGE('',*,*,#2984,.F.);
#3970=ORIENTED_EDGE('',*,*,#2987,.T.);
#3971=ORIENTED_EDGE('',*,*,#2990,.T.);
#3972=ORIENTED_EDGE('',*,*,#2995,.T.);
#3973=ORIENTED_EDGE('',*,*,#3012,.F.);
#3974=ORIENTED_EDGE('',*,*,#3015,.T.);
#3975=ORIENTED_EDGE('',*,*,#3018,.T.);
#3976=ORIENTED_EDGE('',*,*,#3023,.T.);
#3977=ORIENTED_EDGE('',*,*,#3044,.F.);
#3978=ORIENTED_EDGE('',*,*,#3047,.T.);
#3979=ORIENTED_EDGE('',*,*,#3050,.T.);
#3980=ORIENTED_EDGE('',*,*,#3006,.T.);
#3981=ORIENTED_EDGE('',*,*,#2996,.F.);
#3982=ORIENTED_EDGE('',*,*,#3000,.T.);
#3983=ORIENTED_EDGE('',*,*,#3003,.T.);
#3984=ORIENTED_EDGE('',*,*,#3011,.T.);
#3985=ORIENTED_EDGE('',*,*,#3036,.F.);
#3986=ORIENTED_EDGE('',*,*,#3039,.T.);
#3987=ORIENTED_EDGE('',*,*,#3042,.T.);
#3988=ORIENTED_EDGE('',*,*,#2694,.T.);
#3989=ORIENTED_EDGE('',*,*,#2684,.F.);
#3990=ORIENTED_EDGE('',*,*,#2688,.T.);
#3991=ORIENTED_EDGE('',*,*,#2691,.T.);
#3992=ORIENTED_EDGE('',*,*,#2699,.T.);
#3993=ORIENTED_EDGE('',*,*,#2700,.F.);
#3994=ORIENTED_EDGE('',*,*,#2703,.T.);
#3995=ORIENTED_EDGE('',*,*,#2706,.T.);
#3996=ORIENTED_EDGE('',*,*,#2711,.T.);
#3997=ORIENTED_EDGE('',*,*,#2712,.F.);
#3998=ORIENTED_EDGE('',*,*,#2715,.T.);
#3999=ORIENTED_EDGE('',*,*,#2718,.T.);
#4000=ORIENTED_EDGE('',*,*,#2678,.T.);
#4001=ORIENTED_EDGE('',*,*,#2668,.F.);
#4002=ORIENTED_EDGE('',*,*,#2672,.T.);
#4003=ORIENTED_EDGE('',*,*,#2675,.T.);
#4004=ORIENTED_EDGE('',*,*,#2683,.T.);
#4005=ORIENTED_EDGE('',*,*,#2720,.F.);
#4006=ORIENTED_EDGE('',*,*,#2723,.T.);
#4007=ORIENTED_EDGE('',*,*,#2726,.T.);
#4008=ORIENTED_EDGE('',*,*,#2731,.T.);
#4009=ORIENTED_EDGE('',*,*,#2732,.F.);
#4010=ORIENTED_EDGE('',*,*,#2735,.T.);
#4011=ORIENTED_EDGE('',*,*,#2738,.T.);
#4012=ORIENTED_EDGE('',*,*,#2613,.T.);
#4013=ORIENTED_EDGE('',*,*,#2604,.F.);
#4014=ORIENTED_EDGE('',*,*,#2608,.T.);
#4015=ORIENTED_EDGE('',*,*,#2611,.T.);
#4016=ORIENTED_EDGE('',*,*,#2534,.T.);
#4017=ORIENTED_EDGE('',*,*,#2524,.F.);
#4018=ORIENTED_EDGE('',*,*,#2528,.T.);
#4019=ORIENTED_EDGE('',*,*,#2531,.T.);
#4020=ORIENTED_EDGE('',*,*,#2539,.T.);
#4021=ORIENTED_EDGE('',*,*,#2556,.F.);
#4022=ORIENTED_EDGE('',*,*,#2559,.T.);
#4023=ORIENTED_EDGE('',*,*,#2562,.T.);
#4024=ORIENTED_EDGE('',*,*,#2567,.T.);
#4025=ORIENTED_EDGE('',*,*,#2584,.F.);
#4026=ORIENTED_EDGE('',*,*,#2587,.T.);
#4027=ORIENTED_EDGE('',*,*,#2590,.T.);
#4028=ORIENTED_EDGE('',*,*,#2550,.T.);
#4029=ORIENTED_EDGE('',*,*,#2540,.F.);
#4030=ORIENTED_EDGE('',*,*,#2544,.T.);
#4031=ORIENTED_EDGE('',*,*,#2547,.T.);
#4032=ORIENTED_EDGE('',*,*,#2555,.T.);
#4033=ORIENTED_EDGE('',*,*,#2592,.F.);
#4034=ORIENTED_EDGE('',*,*,#2595,.T.);
#4035=ORIENTED_EDGE('',*,*,#2598,.T.);
#4036=ORIENTED_EDGE('',*,*,#2603,.T.);
#4037=ORIENTED_EDGE('',*,*,#2616,.F.);
#4038=ORIENTED_EDGE('',*,*,#2619,.T.);
#4039=ORIENTED_EDGE('',*,*,#2622,.T.);
#4040=ORIENTED_EDGE('',*,*,#2578,.T.);
#4041=ORIENTED_EDGE('',*,*,#2568,.F.);
#4042=ORIENTED_EDGE('',*,*,#2572,.T.);
#4043=ORIENTED_EDGE('',*,*,#2575,.T.);
#4044=ORIENTED_EDGE('',*,*,#2583,.T.);
#4045=ORIENTED_EDGE('',*,*,#2912,.F.);
#4046=ORIENTED_EDGE('',*,*,#2915,.T.);
#4047=ORIENTED_EDGE('',*,*,#2918,.T.);
#4048=ORIENTED_EDGE('',*,*,#2854,.T.);
#4049=ORIENTED_EDGE('',*,*,#2844,.F.);
#4050=ORIENTED_EDGE('',*,*,#2848,.T.);
#4051=ORIENTED_EDGE('',*,*,#2851,.T.);
#4052=ORIENTED_EDGE('',*,*,#2859,.T.);
#4053=ORIENTED_EDGE('',*,*,#2860,.F.);
#4054=ORIENTED_EDGE('',*,*,#2863,.T.);
#4055=ORIENTED_EDGE('',*,*,#2866,.T.);
#4056=ORIENTED_EDGE('',*,*,#2871,.T.);
#4057=ORIENTED_EDGE('',*,*,#2920,.F.);
#4058=ORIENTED_EDGE('',*,*,#2923,.T.);
#4059=ORIENTED_EDGE('',*,*,#2926,.T.);
#4060=ORIENTED_EDGE('',*,*,#2882,.T.);
#4061=ORIENTED_EDGE('',*,*,#2872,.F.);
#4062=ORIENTED_EDGE('',*,*,#2876,.T.);
#4063=ORIENTED_EDGE('',*,*,#2879,.T.);
#4064=ORIENTED_EDGE('',*,*,#2887,.T.);
#4065=ORIENTED_EDGE('',*,*,#2904,.F.);
#4066=ORIENTED_EDGE('',*,*,#2907,.T.);
#4067=ORIENTED_EDGE('',*,*,#2910,.T.);
#4068=ORIENTED_EDGE('',*,*,#2898,.T.);
#4069=ORIENTED_EDGE('',*,*,#2888,.F.);
#4070=ORIENTED_EDGE('',*,*,#2892,.T.);
#4071=ORIENTED_EDGE('',*,*,#2895,.T.);
#4072=ORIENTED_EDGE('',*,*,#2903,.T.);
#4073=ORIENTED_EDGE('',*,*,#2928,.F.);
#4074=ORIENTED_EDGE('',*,*,#2931,.T.);
#4075=ORIENTED_EDGE('',*,*,#2934,.T.);
#4076=ORIENTED_EDGE('',*,*,#2939,.T.);
#4077=ORIENTED_EDGE('',*,*,#3024,.F.);
#4078=ORIENTED_EDGE('',*,*,#3027,.T.);
#4079=ORIENTED_EDGE('',*,*,#3030,.T.);
#4080=ORIENTED_EDGE('',*,*,#3035,.T.);
#4081=ORIENTED_EDGE('',*,*,#3052,.F.);
#4082=ORIENTED_EDGE('',*,*,#3055,.T.);
#4083=ORIENTED_EDGE('',*,*,#3058,.T.);
#4084=ORIENTED_EDGE('',*,*,#2637,.T.);
#4085=ORIENTED_EDGE('',*,*,#2644,.T.);
#4086=ORIENTED_EDGE('',*,*,#2641,.T.);
#4087=ORIENTED_EDGE('',*,*,#2628,.T.);
#4088=ORIENTED_EDGE('',*,*,#2652,.T.);
#4089=ORIENTED_EDGE('',*,*,#3060,.T.);
#4090=ORIENTED_EDGE('',*,*,#2653,.T.);
#4091=ORIENTED_EDGE('',*,*,#2646,.T.);
#4092=ORIENTED_EDGE('',*,*,#2624,.T.);
#4093=ORIENTED_EDGE('',*,*,#2640,.T.);
#4094=ORIENTED_EDGE('',*,*,#2660,.T.);
#4095=ORIENTED_EDGE('',*,*,#2632,.T.);
#4096=ORIENTED_EDGE('',*,*,#2753,.T.);
#4097=ORIENTED_EDGE('',*,*,#2760,.T.);
#4098=ORIENTED_EDGE('',*,*,#2757,.T.);
#4099=ORIENTED_EDGE('',*,*,#2744,.T.);
#4100=ORIENTED_EDGE('',*,*,#2768,.T.);
#4101=ORIENTED_EDGE('',*,*,#2812,.T.);
#4102=ORIENTED_EDGE('',*,*,#2769,.T.);
#4103=ORIENTED_EDGE('',*,*,#2762,.T.);
#4104=ORIENTED_EDGE('',*,*,#2785,.T.);
#4105=ORIENTED_EDGE('',*,*,#2840,.T.);
#4106=ORIENTED_EDGE('',*,*,#2789,.T.);
#4107=ORIENTED_EDGE('',*,*,#2776,.T.);
#4108=ORIENTED_EDGE('',*,*,#2805,.T.);
#4109=ORIENTED_EDGE('',*,*,#2824,.T.);
#4110=ORIENTED_EDGE('',*,*,#2809,.T.);
#4111=ORIENTED_EDGE('',*,*,#2796,.T.);
#4112=ORIENTED_EDGE('',*,*,#2820,.T.);
#4113=ORIENTED_EDGE('',*,*,#2828,.T.);
#4114=ORIENTED_EDGE('',*,*,#2821,.T.);
#4115=ORIENTED_EDGE('',*,*,#2814,.T.);
#4116=ORIENTED_EDGE('',*,*,#2772,.T.);
#4117=ORIENTED_EDGE('',*,*,#2788,.T.);
#4118=ORIENTED_EDGE('',*,*,#2826,.T.);
#4119=ORIENTED_EDGE('',*,*,#2780,.T.);
#4120=ORIENTED_EDGE('',*,*,#2836,.T.);
#4121=ORIENTED_EDGE('',*,*,#2940,.T.);
#4122=ORIENTED_EDGE('',*,*,#2837,.T.);
#4123=ORIENTED_EDGE('',*,*,#2830,.T.);
#4124=ORIENTED_EDGE('',*,*,#2740,.T.);
#4125=ORIENTED_EDGE('',*,*,#2756,.T.);
#4126=ORIENTED_EDGE('',*,*,#2842,.T.);
#4127=ORIENTED_EDGE('',*,*,#2748,.T.);
#4128=ORIENTED_EDGE('',*,*,#2948,.T.);
#4129=ORIENTED_EDGE('',*,*,#2964,.T.);
#4130=ORIENTED_EDGE('',*,*,#2949,.T.);
#4131=ORIENTED_EDGE('',*,*,#2942,.T.);
#4132=ORIENTED_EDGE('',*,*,#2656,.T.);
#4133=ORIENTED_EDGE('',*,*,#2667,.T.);
#4134=ORIENTED_EDGE('',*,*,#2956,.T.);
#4135=ORIENTED_EDGE('',*,*,#2662,.T.);
#4136=ORIENTED_EDGE('',*,*,#2952,.T.);
#4137=ORIENTED_EDGE('',*,*,#2963,.T.);
#4138=ORIENTED_EDGE('',*,*,#2966,.T.);
#4139=ORIENTED_EDGE('',*,*,#2958,.T.);
#4140=ORIENTED_EDGE('',*,*,#3064,.T.);
#4141=ORIENTED_EDGE('',*,*,#2792,.T.);
#4142=ORIENTED_EDGE('',*,*,#2808,.T.);
#4143=ORIENTED_EDGE('',*,*,#3062,.T.);
#4144=ORIENTED_EDGE('',*,*,#2800,.T.);
#4145=ORIENTED_EDGE('',*,*,#3033,.T.);
#4146=ORIENTED_EDGE('',*,*,#3031,.T.);
#4147=ORIENTED_EDGE('',*,*,#3028,.T.);
#4148=ORIENTED_EDGE('',*,*,#3025,.T.);
#4149=ORIENTED_EDGE('',*,*,#2937,.T.);
#4150=ORIENTED_EDGE('',*,*,#2935,.T.);
#4151=ORIENTED_EDGE('',*,*,#2932,.T.);
#4152=ORIENTED_EDGE('',*,*,#2929,.T.);
#4153=ORIENTED_EDGE('',*,*,#2901,.T.);
#4154=ORIENTED_EDGE('',*,*,#2896,.T.);
#4155=ORIENTED_EDGE('',*,*,#2893,.T.);
#4156=ORIENTED_EDGE('',*,*,#2890,.T.);
#4157=ORIENTED_EDGE('',*,*,#2900,.T.);
#4158=ORIENTED_EDGE('',*,*,#2911,.T.);
#4159=ORIENTED_EDGE('',*,*,#2908,.T.);
#4160=ORIENTED_EDGE('',*,*,#2905,.T.);
#4161=ORIENTED_EDGE('',*,*,#2885,.T.);
#4162=ORIENTED_EDGE('',*,*,#2880,.T.);
#4163=ORIENTED_EDGE('',*,*,#2877,.T.);
#4164=ORIENTED_EDGE('',*,*,#2874,.T.);
#4165=ORIENTED_EDGE('',*,*,#2884,.T.);
#4166=ORIENTED_EDGE('',*,*,#2927,.T.);
#4167=ORIENTED_EDGE('',*,*,#2924,.T.);
#4168=ORIENTED_EDGE('',*,*,#2921,.T.);
#4169=ORIENTED_EDGE('',*,*,#2869,.T.);
#4170=ORIENTED_EDGE('',*,*,#2867,.T.);
#4171=ORIENTED_EDGE('',*,*,#2864,.T.);
#4172=ORIENTED_EDGE('',*,*,#2861,.T.);
#4173=ORIENTED_EDGE('',*,*,#2857,.T.);
#4174=ORIENTED_EDGE('',*,*,#2852,.T.);
#4175=ORIENTED_EDGE('',*,*,#2849,.T.);
#4176=ORIENTED_EDGE('',*,*,#2846,.T.);
#4177=ORIENTED_EDGE('',*,*,#2856,.T.);
#4178=ORIENTED_EDGE('',*,*,#2919,.T.);
#4179=ORIENTED_EDGE('',*,*,#2916,.T.);
#4180=ORIENTED_EDGE('',*,*,#2913,.T.);
#4181=ORIENTED_EDGE('',*,*,#2581,.T.);
#4182=ORIENTED_EDGE('',*,*,#2576,.T.);
#4183=ORIENTED_EDGE('',*,*,#2573,.T.);
#4184=ORIENTED_EDGE('',*,*,#2570,.T.);
#4185=ORIENTED_EDGE('',*,*,#2580,.T.);
#4186=ORIENTED_EDGE('',*,*,#2623,.T.);
#4187=ORIENTED_EDGE('',*,*,#2620,.T.);
#4188=ORIENTED_EDGE('',*,*,#2617,.T.);
#4189=ORIENTED_EDGE('',*,*,#2601,.T.);
#4190=ORIENTED_EDGE('',*,*,#2599,.T.);
#4191=ORIENTED_EDGE('',*,*,#2596,.T.);
#4192=ORIENTED_EDGE('',*,*,#2593,.T.);
#4193=ORIENTED_EDGE('',*,*,#2553,.T.);
#4194=ORIENTED_EDGE('',*,*,#2548,.T.);
#4195=ORIENTED_EDGE('',*,*,#2545,.T.);
#4196=ORIENTED_EDGE('',*,*,#2542,.T.);
#4197=ORIENTED_EDGE('',*,*,#2552,.T.);
#4198=ORIENTED_EDGE('',*,*,#2591,.T.);
#4199=ORIENTED_EDGE('',*,*,#2588,.T.);
#4200=ORIENTED_EDGE('',*,*,#2585,.T.);
#4201=ORIENTED_EDGE('',*,*,#2565,.T.);
#4202=ORIENTED_EDGE('',*,*,#2563,.T.);
#4203=ORIENTED_EDGE('',*,*,#2560,.T.);
#4204=ORIENTED_EDGE('',*,*,#2557,.T.);
#4205=ORIENTED_EDGE('',*,*,#2537,.T.);
#4206=ORIENTED_EDGE('',*,*,#2532,.T.);
#4207=ORIENTED_EDGE('',*,*,#2529,.T.);
#4208=ORIENTED_EDGE('',*,*,#2526,.T.);
#4209=ORIENTED_EDGE('',*,*,#2536,.T.);
#4210=ORIENTED_EDGE('',*,*,#2612,.T.);
#4211=ORIENTED_EDGE('',*,*,#2609,.T.);
#4212=ORIENTED_EDGE('',*,*,#2606,.T.);
#4213=ORIENTED_EDGE('',*,*,#2615,.T.);
#4214=ORIENTED_EDGE('',*,*,#2739,.T.);
#4215=ORIENTED_EDGE('',*,*,#2736,.T.);
#4216=ORIENTED_EDGE('',*,*,#2733,.T.);
#4217=ORIENTED_EDGE('',*,*,#2729,.T.);
#4218=ORIENTED_EDGE('',*,*,#2727,.T.);
#4219=ORIENTED_EDGE('',*,*,#2724,.T.);
#4220=ORIENTED_EDGE('',*,*,#2721,.T.);
#4221=ORIENTED_EDGE('',*,*,#2681,.T.);
#4222=ORIENTED_EDGE('',*,*,#2676,.T.);
#4223=ORIENTED_EDGE('',*,*,#2673,.T.);
#4224=ORIENTED_EDGE('',*,*,#2670,.T.);
#4225=ORIENTED_EDGE('',*,*,#2680,.T.);
#4226=ORIENTED_EDGE('',*,*,#2719,.T.);
#4227=ORIENTED_EDGE('',*,*,#2716,.T.);
#4228=ORIENTED_EDGE('',*,*,#2713,.T.);
#4229=ORIENTED_EDGE('',*,*,#2709,.T.);
#4230=ORIENTED_EDGE('',*,*,#2707,.T.);
#4231=ORIENTED_EDGE('',*,*,#2704,.T.);
#4232=ORIENTED_EDGE('',*,*,#2701,.T.);
#4233=ORIENTED_EDGE('',*,*,#2697,.T.);
#4234=ORIENTED_EDGE('',*,*,#2692,.T.);
#4235=ORIENTED_EDGE('',*,*,#2689,.T.);
#4236=ORIENTED_EDGE('',*,*,#2686,.T.);
#4237=ORIENTED_EDGE('',*,*,#2696,.T.);
#4238=ORIENTED_EDGE('',*,*,#3043,.T.);
#4239=ORIENTED_EDGE('',*,*,#3040,.T.);
#4240=ORIENTED_EDGE('',*,*,#3037,.T.);
#4241=ORIENTED_EDGE('',*,*,#3009,.T.);
#4242=ORIENTED_EDGE('',*,*,#3004,.T.);
#4243=ORIENTED_EDGE('',*,*,#3001,.T.);
#4244=ORIENTED_EDGE('',*,*,#2998,.T.);
#4245=ORIENTED_EDGE('',*,*,#3008,.T.);
#4246=ORIENTED_EDGE('',*,*,#3051,.T.);
#4247=ORIENTED_EDGE('',*,*,#3048,.T.);
#4248=ORIENTED_EDGE('',*,*,#3045,.T.);
#4249=ORIENTED_EDGE('',*,*,#3021,.T.);
#4250=ORIENTED_EDGE('',*,*,#3019,.T.);
#4251=ORIENTED_EDGE('',*,*,#3016,.T.);
#4252=ORIENTED_EDGE('',*,*,#3013,.T.);
#4253=ORIENTED_EDGE('',*,*,#2993,.T.);
#4254=ORIENTED_EDGE('',*,*,#2991,.T.);
#4255=ORIENTED_EDGE('',*,*,#2988,.T.);
#4256=ORIENTED_EDGE('',*,*,#2985,.T.);
#4257=ORIENTED_EDGE('',*,*,#2981,.T.);
#4258=ORIENTED_EDGE('',*,*,#2976,.T.);
#4259=ORIENTED_EDGE('',*,*,#2973,.T.);
#4260=ORIENTED_EDGE('',*,*,#2970,.T.);
#4261=ORIENTED_EDGE('',*,*,#2980,.T.);
#4262=ORIENTED_EDGE('',*,*,#3059,.T.);
#4263=ORIENTED_EDGE('',*,*,#3056,.T.);
#4264=ORIENTED_EDGE('',*,*,#3053,.T.);
#4265=ORIENTED_EDGE('',*,*,#2634,.T.);
#4266=ORIENTED_EDGE('',*,*,#2661,.T.);
#4267=ORIENTED_EDGE('',*,*,#2638,.T.);
#4268=ORIENTED_EDGE('',*,*,#2626,.T.);
#4269=ORIENTED_EDGE('',*,*,#2630,.T.);
#4270=ORIENTED_EDGE('',*,*,#2643,.T.);
#4271=ORIENTED_EDGE('',*,*,#2645,.T.);
#4272=ORIENTED_EDGE('',*,*,#2635,.T.);
#4273=ORIENTED_EDGE('',*,*,#2664,.T.);
#4274=ORIENTED_EDGE('',*,*,#2957,.T.);
#4275=ORIENTED_EDGE('',*,*,#2665,.T.);
#4276=ORIENTED_EDGE('',*,*,#2658,.T.);
#4277=ORIENTED_EDGE('',*,*,#2750,.T.);
#4278=ORIENTED_EDGE('',*,*,#2843,.T.);
#4279=ORIENTED_EDGE('',*,*,#2754,.T.);
#4280=ORIENTED_EDGE('',*,*,#2742,.T.);
#4281=ORIENTED_EDGE('',*,*,#2746,.T.);
#4282=ORIENTED_EDGE('',*,*,#2759,.T.);
#4283=ORIENTED_EDGE('',*,*,#2761,.T.);
#4284=ORIENTED_EDGE('',*,*,#2751,.T.);
#4285=ORIENTED_EDGE('',*,*,#2782,.T.);
#4286=ORIENTED_EDGE('',*,*,#2827,.T.);
#4287=ORIENTED_EDGE('',*,*,#2786,.T.);
#4288=ORIENTED_EDGE('',*,*,#2774,.T.);
#4289=ORIENTED_EDGE('',*,*,#2802,.T.);
#4290=ORIENTED_EDGE('',*,*,#3063,.T.);
#4291=ORIENTED_EDGE('',*,*,#2806,.T.);
#4292=ORIENTED_EDGE('',*,*,#2794,.T.);
#4293=ORIENTED_EDGE('',*,*,#2764,.T.);
#4294=ORIENTED_EDGE('',*,*,#2771,.T.);
#4295=ORIENTED_EDGE('',*,*,#2813,.T.);
#4296=ORIENTED_EDGE('',*,*,#2766,.T.);
#4297=ORIENTED_EDGE('',*,*,#2798,.T.);
#4298=ORIENTED_EDGE('',*,*,#2811,.T.);
#4299=ORIENTED_EDGE('',*,*,#2825,.T.);
#4300=ORIENTED_EDGE('',*,*,#2803,.T.);
#4301=ORIENTED_EDGE('',*,*,#2816,.T.);
#4302=ORIENTED_EDGE('',*,*,#2823,.T.);
#4303=ORIENTED_EDGE('',*,*,#2829,.T.);
#4304=ORIENTED_EDGE('',*,*,#2818,.T.);
#4305=ORIENTED_EDGE('',*,*,#2778,.T.);
#4306=ORIENTED_EDGE('',*,*,#2791,.T.);
#4307=ORIENTED_EDGE('',*,*,#2841,.T.);
#4308=ORIENTED_EDGE('',*,*,#2783,.T.);
#4309=ORIENTED_EDGE('',*,*,#2832,.T.);
#4310=ORIENTED_EDGE('',*,*,#2839,.T.);
#4311=ORIENTED_EDGE('',*,*,#2941,.T.);
#4312=ORIENTED_EDGE('',*,*,#2834,.T.);
#4313=ORIENTED_EDGE('',*,*,#2960,.T.);
#4314=ORIENTED_EDGE('',*,*,#2967,.T.);
#4315=ORIENTED_EDGE('',*,*,#2961,.T.);
#4316=ORIENTED_EDGE('',*,*,#2954,.T.);
#4317=ORIENTED_EDGE('',*,*,#2944,.T.);
#4318=ORIENTED_EDGE('',*,*,#2951,.T.);
#4319=ORIENTED_EDGE('',*,*,#2965,.T.);
#4320=ORIENTED_EDGE('',*,*,#2946,.T.);
#4321=ORIENTED_EDGE('',*,*,#3066,.T.);
#4322=ORIENTED_EDGE('',*,*,#2648,.T.);
#4323=ORIENTED_EDGE('',*,*,#2655,.T.);
#4324=ORIENTED_EDGE('',*,*,#3061,.T.);
#4325=ORIENTED_EDGE('',*,*,#2650,.T.);
#4326=ORIENTED_EDGE('',*,*,#3067,.F.);
#4327=ORIENTED_EDGE('',*,*,#3068,.T.);
#4328=ORIENTED_EDGE('',*,*,#3069,.F.);
#4329=ORIENTED_EDGE('',*,*,#3068,.F.);
#4330=ORIENTED_EDGE('',*,*,#3070,.T.);
#4331=ORIENTED_EDGE('',*,*,#3071,.T.);
#4332=ORIENTED_EDGE('',*,*,#3072,.T.);
#4333=ORIENTED_EDGE('',*,*,#3073,.F.);
#4334=ORIENTED_EDGE('',*,*,#3074,.F.);
#4335=ORIENTED_EDGE('',*,*,#3073,.T.);
#4336=ORIENTED_EDGE('',*,*,#3075,.F.);
#4337=ORIENTED_EDGE('',*,*,#3076,.F.);
#4338=ORIENTED_EDGE('',*,*,#3077,.F.);
#4339=ORIENTED_EDGE('',*,*,#3076,.T.);
#4340=ORIENTED_EDGE('',*,*,#3078,.F.);
#4341=ORIENTED_EDGE('',*,*,#3079,.F.);
#4342=ORIENTED_EDGE('',*,*,#3080,.F.);
#4343=ORIENTED_EDGE('',*,*,#3079,.T.);
#4344=ORIENTED_EDGE('',*,*,#3081,.T.);
#4345=ORIENTED_EDGE('',*,*,#3071,.F.);
#4346=ORIENTED_EDGE('',*,*,#3081,.F.);
#4347=ORIENTED_EDGE('',*,*,#3078,.T.);
#4348=ORIENTED_EDGE('',*,*,#3075,.T.);
#4349=ORIENTED_EDGE('',*,*,#3072,.F.);
#4350=ORIENTED_EDGE('',*,*,#3067,.T.);
#4351=ORIENTED_EDGE('',*,*,#3080,.T.);
#4352=ORIENTED_EDGE('',*,*,#3070,.F.);
#4353=ORIENTED_EDGE('',*,*,#3074,.T.);
#4354=ORIENTED_EDGE('',*,*,#3077,.T.);
#4355=ORIENTED_EDGE('',*,*,#3069,.T.);
#4356=ORIENTED_EDGE('',*,*,#3082,.F.);
#4357=ORIENTED_EDGE('',*,*,#3083,.T.);
#4358=ORIENTED_EDGE('',*,*,#3084,.F.);
#4359=ORIENTED_EDGE('',*,*,#3085,.T.);
#4360=ORIENTED_EDGE('',*,*,#3086,.T.);
#4361=ORIENTED_EDGE('',*,*,#3087,.F.);
#4362=ORIENTED_EDGE('',*,*,#3088,.F.);
#4363=ORIENTED_EDGE('',*,*,#3089,.F.);
#4364=ORIENTED_EDGE('',*,*,#3090,.F.);
#4365=ORIENTED_EDGE('',*,*,#3089,.T.);
#4366=ORIENTED_EDGE('',*,*,#3091,.F.);
#4367=ORIENTED_EDGE('',*,*,#3083,.F.);
#4368=ORIENTED_EDGE('',*,*,#3092,.T.);
#4369=ORIENTED_EDGE('',*,*,#3093,.F.);
#4370=ORIENTED_EDGE('',*,*,#3094,.F.);
#4371=ORIENTED_EDGE('',*,*,#3095,.F.);
#4372=ORIENTED_EDGE('',*,*,#3096,.F.);
#4373=ORIENTED_EDGE('',*,*,#3095,.T.);
#4374=ORIENTED_EDGE('',*,*,#3097,.F.);
#4375=ORIENTED_EDGE('',*,*,#3098,.T.);
#4376=ORIENTED_EDGE('',*,*,#3099,.F.);
#4377=ORIENTED_EDGE('',*,*,#3100,.T.);
#4378=ORIENTED_EDGE('',*,*,#3101,.F.);
#4379=ORIENTED_EDGE('',*,*,#3100,.F.);
#4380=ORIENTED_EDGE('',*,*,#3102,.F.);
#4381=ORIENTED_EDGE('',*,*,#3093,.T.);
#4382=ORIENTED_EDGE('',*,*,#3103,.F.);
#4383=ORIENTED_EDGE('',*,*,#3104,.F.);
#4384=ORIENTED_EDGE('',*,*,#3105,.F.);
#4385=ORIENTED_EDGE('',*,*,#3104,.T.);
#4386=ORIENTED_EDGE('',*,*,#3106,.F.);
#4387=ORIENTED_EDGE('',*,*,#3085,.F.);
#4388=ORIENTED_EDGE('',*,*,#3107,.T.);
#4389=ORIENTED_EDGE('',*,*,#3087,.T.);
#4390=ORIENTED_EDGE('',*,*,#3108,.F.);
#4391=ORIENTED_EDGE('',*,*,#3109,.F.);
#4392=ORIENTED_EDGE('',*,*,#3110,.F.);
#4393=ORIENTED_EDGE('',*,*,#3109,.T.);
#4394=ORIENTED_EDGE('',*,*,#3111,.F.);
#4395=ORIENTED_EDGE('',*,*,#3098,.F.);
#4396=ORIENTED_EDGE('',*,*,#3102,.T.);
#4397=ORIENTED_EDGE('',*,*,#3105,.T.);
#4398=ORIENTED_EDGE('',*,*,#3084,.T.);
#4399=ORIENTED_EDGE('',*,*,#3091,.T.);
#4400=ORIENTED_EDGE('',*,*,#3088,.T.);
#4401=ORIENTED_EDGE('',*,*,#3107,.F.);
#4402=ORIENTED_EDGE('',*,*,#3110,.T.);
#4403=ORIENTED_EDGE('',*,*,#3097,.T.);
#4404=ORIENTED_EDGE('',*,*,#3094,.T.);
#4405=ORIENTED_EDGE('',*,*,#3099,.T.);
#4406=ORIENTED_EDGE('',*,*,#3111,.T.);
#4407=ORIENTED_EDGE('',*,*,#3108,.T.);
#4408=ORIENTED_EDGE('',*,*,#3086,.F.);
#4409=ORIENTED_EDGE('',*,*,#3090,.T.);
#4410=ORIENTED_EDGE('',*,*,#3082,.T.);
#4411=ORIENTED_EDGE('',*,*,#3106,.T.);
#4412=ORIENTED_EDGE('',*,*,#3103,.T.);
#4413=ORIENTED_EDGE('',*,*,#3092,.F.);
#4414=ORIENTED_EDGE('',*,*,#3096,.T.);
#4415=ORIENTED_EDGE('',*,*,#3101,.T.);
#4416=ORIENTED_EDGE('',*,*,#3112,.T.);
#4417=ORIENTED_EDGE('',*,*,#3113,.T.);
#4418=ORIENTED_EDGE('',*,*,#3114,.F.);
#4419=ORIENTED_EDGE('',*,*,#3113,.F.);
#4420=ORIENTED_EDGE('',*,*,#3114,.T.);
#4421=ORIENTED_EDGE('',*,*,#3112,.F.);
#4422=ORIENTED_EDGE('',*,*,#3115,.F.);
#4423=ORIENTED_EDGE('',*,*,#3116,.T.);
#4424=ORIENTED_EDGE('',*,*,#3117,.F.);
#4425=ORIENTED_EDGE('',*,*,#3118,.F.);
#4426=ORIENTED_EDGE('',*,*,#3119,.F.);
#4427=ORIENTED_EDGE('',*,*,#3120,.F.);
#4428=ORIENTED_EDGE('',*,*,#3121,.F.);
#4429=ORIENTED_EDGE('',*,*,#3122,.T.);
#4430=ORIENTED_EDGE('',*,*,#3123,.F.);
#4431=ORIENTED_EDGE('',*,*,#3118,.T.);
#4432=ORIENTED_EDGE('',*,*,#3124,.F.);
#4433=ORIENTED_EDGE('',*,*,#3125,.F.);
#4434=ORIENTED_EDGE('',*,*,#3126,.F.);
#4435=ORIENTED_EDGE('',*,*,#3127,.F.);
#4436=ORIENTED_EDGE('',*,*,#3122,.F.);
#4437=ORIENTED_EDGE('',*,*,#3120,.T.);
#4438=ORIENTED_EDGE('',*,*,#3128,.F.);
#4439=ORIENTED_EDGE('',*,*,#3121,.T.);
#4440=ORIENTED_EDGE('',*,*,#3129,.T.);
#4441=ORIENTED_EDGE('',*,*,#3115,.T.);
#4442=ORIENTED_EDGE('',*,*,#3129,.F.);
#4443=ORIENTED_EDGE('',*,*,#3124,.T.);
#4444=ORIENTED_EDGE('',*,*,#3117,.T.);
#4445=ORIENTED_EDGE('',*,*,#3128,.T.);
#4446=ORIENTED_EDGE('',*,*,#3119,.T.);
#4447=ORIENTED_EDGE('',*,*,#3123,.T.);
#4448=ORIENTED_EDGE('',*,*,#3127,.T.);
#4449=ORIENTED_EDGE('',*,*,#3130,.T.);
#4450=ORIENTED_EDGE('',*,*,#3125,.T.);
#4451=ORIENTED_EDGE('',*,*,#3126,.T.);
#4452=ORIENTED_EDGE('',*,*,#3130,.F.);
#4453=ORIENTED_EDGE('',*,*,#3131,.T.);
#4454=ORIENTED_EDGE('',*,*,#3116,.F.);
#4455=ORIENTED_EDGE('',*,*,#3132,.T.);
#4456=ORIENTED_EDGE('',*,*,#3131,.F.);
#4457=ORIENTED_EDGE('',*,*,#3132,.F.);
#4458=ORIENTED_EDGE('',*,*,#3133,.F.);
#4459=ORIENTED_EDGE('',*,*,#3134,.T.);
#4460=ORIENTED_EDGE('',*,*,#3135,.T.);
#4461=ORIENTED_EDGE('',*,*,#3134,.F.);
#4462=ORIENTED_EDGE('',*,*,#3133,.T.);
#4463=ORIENTED_EDGE('',*,*,#3135,.F.);
#4464=ORIENTED_EDGE('',*,*,#3136,.F.);
#4465=ORIENTED_EDGE('',*,*,#3137,.T.);
#4466=ORIENTED_EDGE('',*,*,#3138,.T.);
#4467=ORIENTED_EDGE('',*,*,#3137,.F.);
#4468=ORIENTED_EDGE('',*,*,#3139,.F.);
#4469=ORIENTED_EDGE('',*,*,#3140,.T.);
#4470=ORIENTED_EDGE('',*,*,#3141,.T.);
#4471=ORIENTED_EDGE('',*,*,#3140,.F.);
#4472=ORIENTED_EDGE('',*,*,#3142,.F.);
#4473=ORIENTED_EDGE('',*,*,#3143,.F.);
#4474=ORIENTED_EDGE('',*,*,#3144,.T.);
#4475=ORIENTED_EDGE('',*,*,#3145,.T.);
#4476=ORIENTED_EDGE('',*,*,#3144,.F.);
#4477=ORIENTED_EDGE('',*,*,#3142,.T.);
#4478=ORIENTED_EDGE('',*,*,#3143,.T.);
#4479=ORIENTED_EDGE('',*,*,#3146,.T.);
#4480=ORIENTED_EDGE('',*,*,#3147,.F.);
#4481=ORIENTED_EDGE('',*,*,#3146,.F.);
#4482=ORIENTED_EDGE('',*,*,#3148,.F.);
#4483=ORIENTED_EDGE('',*,*,#3149,.T.);
#4484=ORIENTED_EDGE('',*,*,#3150,.T.);
#4485=ORIENTED_EDGE('',*,*,#3149,.F.);
#4486=ORIENTED_EDGE('',*,*,#3151,.F.);
#4487=ORIENTED_EDGE('',*,*,#3152,.T.);
#4488=ORIENTED_EDGE('',*,*,#3148,.T.);
#4489=ORIENTED_EDGE('',*,*,#3152,.F.);
#4490=ORIENTED_EDGE('',*,*,#3153,.F.);
#4491=ORIENTED_EDGE('',*,*,#3154,.T.);
#4492=ORIENTED_EDGE('',*,*,#3151,.T.);
#4493=ORIENTED_EDGE('',*,*,#3154,.F.);
#4494=ORIENTED_EDGE('',*,*,#3138,.F.);
#4495=ORIENTED_EDGE('',*,*,#3155,.T.);
#4496=ORIENTED_EDGE('',*,*,#3156,.T.);
#4497=ORIENTED_EDGE('',*,*,#3155,.F.);
#4498=ORIENTED_EDGE('',*,*,#3153,.T.);
#4499=ORIENTED_EDGE('',*,*,#3156,.F.);
#4500=ORIENTED_EDGE('',*,*,#3150,.F.);
#4501=ORIENTED_EDGE('',*,*,#3147,.T.);
#4502=ORIENTED_EDGE('',*,*,#3139,.T.);
#4503=ORIENTED_EDGE('',*,*,#3145,.F.);
#4504=ORIENTED_EDGE('',*,*,#3141,.F.);
#4505=ORIENTED_EDGE('',*,*,#3136,.T.);
#4506=ORIENTED_EDGE('',*,*,#3157,.T.);
#4507=ORIENTED_EDGE('',*,*,#3158,.T.);
#4508=ORIENTED_EDGE('',*,*,#3159,.F.);
#4509=ORIENTED_EDGE('',*,*,#3158,.F.);
#4510=ORIENTED_EDGE('',*,*,#3160,.T.);
#4511=ORIENTED_EDGE('',*,*,#3157,.F.);
#4512=ORIENTED_EDGE('',*,*,#3161,.T.);
#4513=ORIENTED_EDGE('',*,*,#3162,.T.);
#4514=ORIENTED_EDGE('',*,*,#3161,.F.);
#4515=ORIENTED_EDGE('',*,*,#3160,.F.);
#4516=ORIENTED_EDGE('',*,*,#3162,.F.);
#4517=ORIENTED_EDGE('',*,*,#3163,.T.);
#4518=ORIENTED_EDGE('',*,*,#3164,.T.);
#4519=ORIENTED_EDGE('',*,*,#3163,.F.);
#4520=ORIENTED_EDGE('',*,*,#3165,.F.);
#4521=ORIENTED_EDGE('',*,*,#3166,.T.);
#4522=ORIENTED_EDGE('',*,*,#3167,.T.);
#4523=ORIENTED_EDGE('',*,*,#3166,.F.);
#4524=ORIENTED_EDGE('',*,*,#3168,.F.);
#4525=ORIENTED_EDGE('',*,*,#3169,.T.);
#4526=ORIENTED_EDGE('',*,*,#3170,.T.);
#4527=ORIENTED_EDGE('',*,*,#3169,.F.);
#4528=ORIENTED_EDGE('',*,*,#3170,.F.);
#4529=ORIENTED_EDGE('',*,*,#3171,.T.);
#4530=ORIENTED_EDGE('',*,*,#3172,.T.);
#4531=ORIENTED_EDGE('',*,*,#3171,.F.);
#4532=ORIENTED_EDGE('',*,*,#3172,.F.);
#4533=ORIENTED_EDGE('',*,*,#3173,.T.);
#4534=ORIENTED_EDGE('',*,*,#3174,.T.);
#4535=ORIENTED_EDGE('',*,*,#3173,.F.);
#4536=ORIENTED_EDGE('',*,*,#3175,.F.);
#4537=ORIENTED_EDGE('',*,*,#3176,.T.);
#4538=ORIENTED_EDGE('',*,*,#3177,.T.);
#4539=ORIENTED_EDGE('',*,*,#3176,.F.);
#4540=ORIENTED_EDGE('',*,*,#3177,.F.);
#4541=ORIENTED_EDGE('',*,*,#3178,.T.);
#4542=ORIENTED_EDGE('',*,*,#3179,.T.);
#4543=ORIENTED_EDGE('',*,*,#3178,.F.);
#4544=ORIENTED_EDGE('',*,*,#3179,.F.);
#4545=ORIENTED_EDGE('',*,*,#3180,.T.);
#4546=ORIENTED_EDGE('',*,*,#3181,.T.);
#4547=ORIENTED_EDGE('',*,*,#3180,.F.);
#4548=ORIENTED_EDGE('',*,*,#3174,.F.);
#4549=ORIENTED_EDGE('',*,*,#3175,.T.);
#4550=ORIENTED_EDGE('',*,*,#3167,.F.);
#4551=ORIENTED_EDGE('',*,*,#3168,.T.);
#4552=ORIENTED_EDGE('',*,*,#3165,.T.);
#4553=ORIENTED_EDGE('',*,*,#3164,.F.);
#4554=ORIENTED_EDGE('',*,*,#3159,.T.);
#4555=ORIENTED_EDGE('',*,*,#3181,.F.);
#4556=ORIENTED_EDGE('',*,*,#3182,.F.);
#4557=ORIENTED_EDGE('',*,*,#3183,.T.);
#4558=ORIENTED_EDGE('',*,*,#3184,.T.);
#4559=ORIENTED_EDGE('',*,*,#3183,.F.);
#4560=ORIENTED_EDGE('',*,*,#3185,.F.);
#4561=ORIENTED_EDGE('',*,*,#3186,.T.);
#4562=ORIENTED_EDGE('',*,*,#3187,.T.);
#4563=ORIENTED_EDGE('',*,*,#3186,.F.);
#4564=ORIENTED_EDGE('',*,*,#3188,.F.);
#4565=ORIENTED_EDGE('',*,*,#3189,.T.);
#4566=ORIENTED_EDGE('',*,*,#3185,.T.);
#4567=ORIENTED_EDGE('',*,*,#3189,.F.);
#4568=ORIENTED_EDGE('',*,*,#3190,.F.);
#4569=ORIENTED_EDGE('',*,*,#3191,.T.);
#4570=ORIENTED_EDGE('',*,*,#3188,.T.);
#4571=ORIENTED_EDGE('',*,*,#3191,.F.);
#4572=ORIENTED_EDGE('',*,*,#3192,.F.);
#4573=ORIENTED_EDGE('',*,*,#3193,.T.);
#4574=ORIENTED_EDGE('',*,*,#3194,.T.);
#4575=ORIENTED_EDGE('',*,*,#3193,.F.);
#4576=ORIENTED_EDGE('',*,*,#3195,.F.);
#4577=ORIENTED_EDGE('',*,*,#3196,.T.);
#4578=ORIENTED_EDGE('',*,*,#3192,.T.);
#4579=ORIENTED_EDGE('',*,*,#3196,.F.);
#4580=ORIENTED_EDGE('',*,*,#3197,.F.);
#4581=ORIENTED_EDGE('',*,*,#3198,.T.);
#4582=ORIENTED_EDGE('',*,*,#3195,.T.);
#4583=ORIENTED_EDGE('',*,*,#3198,.F.);
#4584=ORIENTED_EDGE('',*,*,#3199,.F.);
#4585=ORIENTED_EDGE('',*,*,#3200,.T.);
#4586=ORIENTED_EDGE('',*,*,#3201,.T.);
#4587=ORIENTED_EDGE('',*,*,#3200,.F.);
#4588=ORIENTED_EDGE('',*,*,#3202,.F.);
#4589=ORIENTED_EDGE('',*,*,#3203,.T.);
#4590=ORIENTED_EDGE('',*,*,#3199,.T.);
#4591=ORIENTED_EDGE('',*,*,#3203,.F.);
#4592=ORIENTED_EDGE('',*,*,#3204,.F.);
#4593=ORIENTED_EDGE('',*,*,#3205,.T.);
#4594=ORIENTED_EDGE('',*,*,#3202,.T.);
#4595=ORIENTED_EDGE('',*,*,#3205,.F.);
#4596=ORIENTED_EDGE('',*,*,#3206,.F.);
#4597=ORIENTED_EDGE('',*,*,#3207,.T.);
#4598=ORIENTED_EDGE('',*,*,#3208,.T.);
#4599=ORIENTED_EDGE('',*,*,#3207,.F.);
#4600=ORIENTED_EDGE('',*,*,#3209,.F.);
#4601=ORIENTED_EDGE('',*,*,#3210,.T.);
#4602=ORIENTED_EDGE('',*,*,#3206,.T.);
#4603=ORIENTED_EDGE('',*,*,#3210,.F.);
#4604=ORIENTED_EDGE('',*,*,#3209,.T.);
#4605=ORIENTED_EDGE('',*,*,#3184,.F.);
#4606=ORIENTED_EDGE('',*,*,#3204,.T.);
#4607=ORIENTED_EDGE('',*,*,#3208,.F.);
#4608=ORIENTED_EDGE('',*,*,#3197,.T.);
#4609=ORIENTED_EDGE('',*,*,#3201,.F.);
#4610=ORIENTED_EDGE('',*,*,#3194,.F.);
#4611=ORIENTED_EDGE('',*,*,#3190,.T.);
#4612=ORIENTED_EDGE('',*,*,#3187,.F.);
#4613=ORIENTED_EDGE('',*,*,#3182,.T.);
#4614=ORIENTED_EDGE('',*,*,#3211,.T.);
#4615=ORIENTED_EDGE('',*,*,#3212,.T.);
#4616=ORIENTED_EDGE('',*,*,#3213,.F.);
#4617=ORIENTED_EDGE('',*,*,#3212,.F.);
#4618=ORIENTED_EDGE('',*,*,#3214,.T.);
#4619=ORIENTED_EDGE('',*,*,#3215,.T.);
#4620=ORIENTED_EDGE('',*,*,#3216,.F.);
#4621=ORIENTED_EDGE('',*,*,#3215,.F.);
#4622=ORIENTED_EDGE('',*,*,#3217,.T.);
#4623=ORIENTED_EDGE('',*,*,#3218,.T.);
#4624=ORIENTED_EDGE('',*,*,#3214,.F.);
#4625=ORIENTED_EDGE('',*,*,#3218,.F.);
#4626=ORIENTED_EDGE('',*,*,#3219,.T.);
#4627=ORIENTED_EDGE('',*,*,#3220,.T.);
#4628=ORIENTED_EDGE('',*,*,#3217,.F.);
#4629=ORIENTED_EDGE('',*,*,#3220,.F.);
#4630=ORIENTED_EDGE('',*,*,#3221,.T.);
#4631=ORIENTED_EDGE('',*,*,#3222,.T.);
#4632=ORIENTED_EDGE('',*,*,#3223,.F.);
#4633=ORIENTED_EDGE('',*,*,#3222,.F.);
#4634=ORIENTED_EDGE('',*,*,#3224,.T.);
#4635=ORIENTED_EDGE('',*,*,#3225,.T.);
#4636=ORIENTED_EDGE('',*,*,#3221,.F.);
#4637=ORIENTED_EDGE('',*,*,#3225,.F.);
#4638=ORIENTED_EDGE('',*,*,#3226,.T.);
#4639=ORIENTED_EDGE('',*,*,#3227,.T.);
#4640=ORIENTED_EDGE('',*,*,#3224,.F.);
#4641=ORIENTED_EDGE('',*,*,#3227,.F.);
#4642=ORIENTED_EDGE('',*,*,#3228,.T.);
#4643=ORIENTED_EDGE('',*,*,#3229,.T.);
#4644=ORIENTED_EDGE('',*,*,#3230,.F.);
#4645=ORIENTED_EDGE('',*,*,#3229,.F.);
#4646=ORIENTED_EDGE('',*,*,#3231,.T.);
#4647=ORIENTED_EDGE('',*,*,#3232,.T.);
#4648=ORIENTED_EDGE('',*,*,#3228,.F.);
#4649=ORIENTED_EDGE('',*,*,#3232,.F.);
#4650=ORIENTED_EDGE('',*,*,#3233,.T.);
#4651=ORIENTED_EDGE('',*,*,#3234,.T.);
#4652=ORIENTED_EDGE('',*,*,#3231,.F.);
#4653=ORIENTED_EDGE('',*,*,#3234,.F.);
#4654=ORIENTED_EDGE('',*,*,#3235,.T.);
#4655=ORIENTED_EDGE('',*,*,#3236,.T.);
#4656=ORIENTED_EDGE('',*,*,#3237,.F.);
#4657=ORIENTED_EDGE('',*,*,#3236,.F.);
#4658=ORIENTED_EDGE('',*,*,#3238,.T.);
#4659=ORIENTED_EDGE('',*,*,#3239,.T.);
#4660=ORIENTED_EDGE('',*,*,#3235,.F.);
#4661=ORIENTED_EDGE('',*,*,#3239,.F.);
#4662=ORIENTED_EDGE('',*,*,#3238,.F.);
#4663=ORIENTED_EDGE('',*,*,#3213,.T.);
#4664=ORIENTED_EDGE('',*,*,#3233,.F.);
#4665=ORIENTED_EDGE('',*,*,#3237,.T.);
#4666=ORIENTED_EDGE('',*,*,#3226,.F.);
#4667=ORIENTED_EDGE('',*,*,#3230,.T.);
#4668=ORIENTED_EDGE('',*,*,#3223,.T.);
#4669=ORIENTED_EDGE('',*,*,#3219,.F.);
#4670=ORIENTED_EDGE('',*,*,#3216,.T.);
#4671=ORIENTED_EDGE('',*,*,#3211,.F.);
#4672=PLANE('',#5204);
#4673=PLANE('',#5205);
#4674=PLANE('',#5206);
#4675=PLANE('',#5213);
#4676=PLANE('',#5214);
#4677=PLANE('',#5215);
#4678=PLANE('',#5222);
#4679=PLANE('',#5223);
#4680=PLANE('',#5224);
#4681=PLANE('',#5228);
#4682=PLANE('',#5229);
#4683=PLANE('',#5230);
#4684=PLANE('',#5237);
#4685=PLANE('',#5238);
#4686=PLANE('',#5239);
#4687=PLANE('',#5240);
#4688=PLANE('',#5241);
#4689=PLANE('',#5242);
#4690=PLANE('',#5246);
#4691=PLANE('',#5247);
#4692=PLANE('',#5248);
#4693=PLANE('',#5252);
#4694=PLANE('',#5253);
#4695=PLANE('',#5254);
#4696=PLANE('',#5255);
#4697=PLANE('',#5256);
#4698=PLANE('',#5269);
#4699=PLANE('',#5270);
#4700=PLANE('',#5277);
#4701=PLANE('',#5278);
#4702=PLANE('',#5285);
#4703=PLANE('',#5286);
#4704=PLANE('',#5287);
#4705=PLANE('',#5294);
#4706=PLANE('',#5295);
#4707=PLANE('',#5296);
#4708=PLANE('',#5303);
#4709=PLANE('',#5304);
#4710=PLANE('',#5305);
#4711=PLANE('',#5309);
#4712=PLANE('',#5310);
#4713=PLANE('',#5311);
#4714=PLANE('',#5312);
#4715=PLANE('',#5313);
#4716=PLANE('',#5314);
#4717=PLANE('',#5318);
#4718=PLANE('',#5319);
#4719=PLANE('',#5320);
#4720=PLANE('',#5321);
#4721=PLANE('',#5322);
#4722=PLANE('',#5335);
#4723=PLANE('',#5336);
#4724=PLANE('',#5343);
#4725=PLANE('',#5344);
#4726=PLANE('',#5357);
#4727=PLANE('',#5358);
#4728=PLANE('',#5371);
#4729=PLANE('',#5372);
#4730=PLANE('',#5379);
#4731=PLANE('',#5380);
#4732=PLANE('',#5381);
#4733=PLANE('',#5382);
#4734=PLANE('',#5389);
#4735=PLANE('',#5390);
#4736=PLANE('',#5391);
#4737=PLANE('',#5392);
#4738=PLANE('',#5393);
#4739=PLANE('',#5400);
#4740=PLANE('',#5401);
#4741=PLANE('',#5402);
#4742=PLANE('',#5406);
#4743=PLANE('',#5407);
#4744=PLANE('',#5408);
#4745=PLANE('',#5415);
#4746=PLANE('',#5416);
#4747=PLANE('',#5417);
#4748=PLANE('',#5424);
#4749=PLANE('',#5425);
#4750=PLANE('',#5426);
#4751=PLANE('',#5427);
#4752=PLANE('',#5428);
#4753=PLANE('',#5429);
#4754=PLANE('',#5430);
#4755=PLANE('',#5431);
#4756=PLANE('',#5432);
#4757=PLANE('',#5433);
#4758=PLANE('',#5434);
#4759=PLANE('',#5435);
#4760=PLANE('',#5439);
#4761=PLANE('',#5440);
#4762=PLANE('',#5447);
#4763=PLANE('',#5448);
#4764=PLANE('',#5455);
#4765=PLANE('',#5456);
#4766=PLANE('',#5457);
#4767=PLANE('',#5458);
#4768=PLANE('',#5459);
#4769=PLANE('',#5466);
#4770=PLANE('',#5467);
#4771=PLANE('',#5468);
#4772=PLANE('',#5472);
#4773=PLANE('',#5473);
#4774=PLANE('',#5474);
#4775=PLANE('',#5481);
#4776=PLANE('',#5482);
#4777=PLANE('',#5483);
#4778=PLANE('',#5487);
#4779=PLANE('',#5488);
#4780=PLANE('',#5489);
#4781=PLANE('',#5493);
#4782=PLANE('',#5494);
#4783=PLANE('',#5495);
#4784=PLANE('',#5496);
#4785=PLANE('',#5497);
#4786=PLANE('',#5498);
#4787=PLANE('',#5499);
#4788=PLANE('',#5500);
#4789=PLANE('',#5501);
#4790=PLANE('',#5502);
#4791=PLANE('',#5503);
#4792=PLANE('',#5507);
#4793=PLANE('',#5508);
#4794=PLANE('',#5513);
#4795=PLANE('',#5514);
#4796=PLANE('',#5515);
#4797=PLANE('',#5516);
#4798=PLANE('',#5517);
#4799=PLANE('',#5518);
#4800=PLANE('',#5520);
#4801=PLANE('',#5521);
#4802=PLANE('',#5525);
#4803=PLANE('',#5526);
#4804=PLANE('',#5530);
#4805=PLANE('',#5534);
#4806=PLANE('',#5538);
#4807=PLANE('',#5539);
#4808=PLANE('',#5544);
#4809=PLANE('',#5545);
#4810=PLANE('',#5547);
#4811=PLANE('',#5550);
#4812=PLANE('',#5551);
#4813=PLANE('',#5555);
#4814=PLANE('',#5556);
#4815=PLANE('',#5561);
#4816=PLANE('',#5562);
#4817=PLANE('',#5569);
#4818=PLANE('',#5570);
#4819=PLANE('',#5595);
#4820=PLANE('',#5596);
#4821=PLANE('',#5597);
#4822=PLANE('',#5598);
#4823=PLANE('',#5628);
#4824=PLANE('',#5629);
#4825=PLANE('',#5630);
#4826=PLANE('',#5631);
#4827=PLANE('',#5668);
#4828=PLANE('',#5669);
#4829=PLANE('',#5670);
#4830=PLANE('',#5671);
#4831=PLANE('',#5672);
#4832=PLANE('',#5709);
#4833=PLANE('',#5710);
#4834=PLANE('',#5711);
#4835=PLANE('',#5712);
#4836=PLANE('',#5713);
#4837=ADVANCED_FACE('',(#475),#4672,.T.);
#4838=ADVANCED_FACE('',(#476),#4673,.T.);
#4839=ADVANCED_FACE('',(#477),#4674,.T.);
#4840=ADVANCED_FACE('',(#478),#396,.T.);
#4841=ADVANCED_FACE('',(#479),#397,.T.);
#4842=ADVANCED_FACE('',(#480),#4675,.T.);
#4843=ADVANCED_FACE('',(#481),#4676,.T.);
#4844=ADVANCED_FACE('',(#482),#4677,.T.);
#4845=ADVANCED_FACE('',(#483),#398,.T.);
#4846=ADVANCED_FACE('',(#484),#399,.T.);
#4847=ADVANCED_FACE('',(#485),#4678,.T.);
#4848=ADVANCED_FACE('',(#486),#4679,.T.);
#4849=ADVANCED_FACE('',(#487),#4680,.T.);
#4850=ADVANCED_FACE('',(#488),#400,.T.);
#4851=ADVANCED_FACE('',(#489),#4681,.T.);
#4852=ADVANCED_FACE('',(#490),#4682,.T.);
#4853=ADVANCED_FACE('',(#491),#4683,.T.);
#4854=ADVANCED_FACE('',(#492),#401,.T.);
#4855=ADVANCED_FACE('',(#493),#402,.T.);
#4856=ADVANCED_FACE('',(#494),#4684,.T.);
#4857=ADVANCED_FACE('',(#495),#4685,.T.);
#4858=ADVANCED_FACE('',(#496),#4686,.T.);
#4859=ADVANCED_FACE('',(#497),#4687,.T.);
#4860=ADVANCED_FACE('',(#498),#4688,.T.);
#4861=ADVANCED_FACE('',(#499),#4689,.T.);
#4862=ADVANCED_FACE('',(#500),#403,.T.);
#4863=ADVANCED_FACE('',(#501),#4690,.T.);
#4864=ADVANCED_FACE('',(#502),#4691,.T.);
#4865=ADVANCED_FACE('',(#503),#4692,.T.);
#4866=ADVANCED_FACE('',(#504),#404,.T.);
#4867=ADVANCED_FACE('',(#505),#4693,.T.);
#4868=ADVANCED_FACE('',(#506),#4694,.T.);
#4869=ADVANCED_FACE('',(#507),#4695,.T.);
#4870=ADVANCED_FACE('',(#508),#4696,.T.);
#4871=ADVANCED_FACE('',(#509),#4697,.T.);
#4872=ADVANCED_FACE('',(#510),#405,.F.);
#4873=ADVANCED_FACE('',(#511),#406,.F.);
#4874=ADVANCED_FACE('',(#512),#407,.T.);
#4875=ADVANCED_FACE('',(#513),#408,.T.);
#4876=ADVANCED_FACE('',(#514),#4698,.T.);
#4877=ADVANCED_FACE('',(#515),#4699,.T.);
#4878=ADVANCED_FACE('',(#516),#409,.F.);
#4879=ADVANCED_FACE('',(#517),#410,.T.);
#4880=ADVANCED_FACE('',(#518),#4700,.T.);
#4881=ADVANCED_FACE('',(#519),#4701,.T.);
#4882=ADVANCED_FACE('',(#520),#411,.F.);
#4883=ADVANCED_FACE('',(#521),#412,.T.);
#4884=ADVANCED_FACE('',(#522),#4702,.T.);
#4885=ADVANCED_FACE('',(#523),#4703,.T.);
#4886=ADVANCED_FACE('',(#524),#4704,.T.);
#4887=ADVANCED_FACE('',(#525),#413,.T.);
#4888=ADVANCED_FACE('',(#526),#414,.T.);
#4889=ADVANCED_FACE('',(#527),#4705,.T.);
#4890=ADVANCED_FACE('',(#528),#4706,.T.);
#4891=ADVANCED_FACE('',(#529),#4707,.T.);
#4892=ADVANCED_FACE('',(#530),#415,.T.);
#4893=ADVANCED_FACE('',(#531),#416,.T.);
#4894=ADVANCED_FACE('',(#532),#4708,.T.);
#4895=ADVANCED_FACE('',(#533),#4709,.T.);
#4896=ADVANCED_FACE('',(#534),#4710,.T.);
#4897=ADVANCED_FACE('',(#535),#417,.T.);
#4898=ADVANCED_FACE('',(#536),#4711,.T.);
#4899=ADVANCED_FACE('',(#537),#4712,.T.);
#4900=ADVANCED_FACE('',(#538),#4713,.T.);
#4901=ADVANCED_FACE('',(#539),#4714,.T.);
#4902=ADVANCED_FACE('',(#540),#4715,.T.);
#4903=ADVANCED_FACE('',(#541),#4716,.T.);
#4904=ADVANCED_FACE('',(#542),#418,.T.);
#4905=ADVANCED_FACE('',(#543),#4717,.T.);
#4906=ADVANCED_FACE('',(#544),#4718,.T.);
#4907=ADVANCED_FACE('',(#545),#4719,.T.);
#4908=ADVANCED_FACE('',(#546),#4720,.T.);
#4909=ADVANCED_FACE('',(#547),#4721,.T.);
#4910=ADVANCED_FACE('',(#548),#419,.F.);
#4911=ADVANCED_FACE('',(#549),#420,.F.);
#4912=ADVANCED_FACE('',(#550),#421,.T.);
#4913=ADVANCED_FACE('',(#551),#422,.T.);
#4914=ADVANCED_FACE('',(#552),#4722,.T.);
#4915=ADVANCED_FACE('',(#553),#4723,.T.);
#4916=ADVANCED_FACE('',(#554),#423,.F.);
#4917=ADVANCED_FACE('',(#555),#424,.T.);
#4918=ADVANCED_FACE('',(#556),#4724,.T.);
#4919=ADVANCED_FACE('',(#557),#4725,.T.);
#4920=ADVANCED_FACE('',(#558),#425,.F.);
#4921=ADVANCED_FACE('',(#559),#426,.F.);
#4922=ADVANCED_FACE('',(#560),#427,.T.);
#4923=ADVANCED_FACE('',(#561),#428,.T.);
#4924=ADVANCED_FACE('',(#562),#4726,.T.);
#4925=ADVANCED_FACE('',(#563),#4727,.T.);
#4926=ADVANCED_FACE('',(#564),#429,.F.);
#4927=ADVANCED_FACE('',(#565),#430,.F.);
#4928=ADVANCED_FACE('',(#566),#431,.T.);
#4929=ADVANCED_FACE('',(#567),#432,.T.);
#4930=ADVANCED_FACE('',(#568),#4728,.T.);
#4931=ADVANCED_FACE('',(#569),#4729,.T.);
#4932=ADVANCED_FACE('',(#570),#433,.F.);
#4933=ADVANCED_FACE('',(#571),#434,.T.);
#4934=ADVANCED_FACE('',(#572),#4730,.T.);
#4935=ADVANCED_FACE('',(#573),#4731,.T.);
#4936=ADVANCED_FACE('',(#574),#4732,.T.);
#4937=ADVANCED_FACE('',(#575),#4733,.T.);
#4938=ADVANCED_FACE('',(#576),#435,.F.);
#4939=ADVANCED_FACE('',(#577),#436,.T.);
#4940=ADVANCED_FACE('',(#578),#4734,.T.);
#4941=ADVANCED_FACE('',(#579),#4735,.T.);
#4942=ADVANCED_FACE('',(#580),#4736,.T.);
#4943=ADVANCED_FACE('',(#581),#4737,.T.);
#4944=ADVANCED_FACE('',(#582),#4738,.T.);
#4945=ADVANCED_FACE('',(#583),#437,.T.);
#4946=ADVANCED_FACE('',(#584),#438,.T.);
#4947=ADVANCED_FACE('',(#585),#4739,.T.);
#4948=ADVANCED_FACE('',(#586),#4740,.T.);
#4949=ADVANCED_FACE('',(#587),#4741,.T.);
#4950=ADVANCED_FACE('',(#588),#439,.T.);
#4951=ADVANCED_FACE('',(#589),#4742,.T.);
#4952=ADVANCED_FACE('',(#590),#4743,.T.);
#4953=ADVANCED_FACE('',(#591),#4744,.T.);
#4954=ADVANCED_FACE('',(#592),#440,.T.);
#4955=ADVANCED_FACE('',(#593),#441,.T.);
#4956=ADVANCED_FACE('',(#594),#4745,.T.);
#4957=ADVANCED_FACE('',(#595),#4746,.T.);
#4958=ADVANCED_FACE('',(#596),#4747,.T.);
#4959=ADVANCED_FACE('',(#597),#442,.T.);
#4960=ADVANCED_FACE('',(#598),#443,.T.);
#4961=ADVANCED_FACE('',(#599),#4748,.T.);
#4962=ADVANCED_FACE('',(#600),#4749,.T.);
#4963=ADVANCED_FACE('',(#601),#4750,.T.);
#4964=ADVANCED_FACE('',(#602),#4751,.T.);
#4965=ADVANCED_FACE('',(#603),#4752,.T.);
#4966=ADVANCED_FACE('',(#604),#4753,.T.);
#4967=ADVANCED_FACE('',(#605),#4754,.T.);
#4968=ADVANCED_FACE('',(#606),#4755,.T.);
#4969=ADVANCED_FACE('',(#607),#4756,.T.);
#4970=ADVANCED_FACE('',(#608),#4757,.T.);
#4971=ADVANCED_FACE('',(#609),#4758,.T.);
#4972=ADVANCED_FACE('',(#610),#4759,.T.);
#4973=ADVANCED_FACE('',(#611),#444,.T.);
#4974=ADVANCED_FACE('',(#612),#4760,.T.);
#4975=ADVANCED_FACE('',(#613),#4761,.T.);
#4976=ADVANCED_FACE('',(#614),#445,.F.);
#4977=ADVANCED_FACE('',(#615),#446,.T.);
#4978=ADVANCED_FACE('',(#616),#4762,.T.);
#4979=ADVANCED_FACE('',(#617),#4763,.T.);
#4980=ADVANCED_FACE('',(#618),#447,.F.);
#4981=ADVANCED_FACE('',(#619),#448,.T.);
#4982=ADVANCED_FACE('',(#620),#4764,.T.);
#4983=ADVANCED_FACE('',(#621),#4765,.T.);
#4984=ADVANCED_FACE('',(#622),#4766,.T.);
#4985=ADVANCED_FACE('',(#623),#4767,.T.);
#4986=ADVANCED_FACE('',(#624),#4768,.T.);
#4987=ADVANCED_FACE('',(#625),#449,.T.);
#4988=ADVANCED_FACE('',(#626),#450,.T.);
#4989=ADVANCED_FACE('',(#627),#4769,.T.);
#4990=ADVANCED_FACE('',(#628),#4770,.T.);
#4991=ADVANCED_FACE('',(#629),#4771,.T.);
#4992=ADVANCED_FACE('',(#630),#451,.T.);
#4993=ADVANCED_FACE('',(#631),#4772,.T.);
#4994=ADVANCED_FACE('',(#632),#4773,.T.);
#4995=ADVANCED_FACE('',(#633),#4774,.T.);
#4996=ADVANCED_FACE('',(#634),#452,.T.);
#4997=ADVANCED_FACE('',(#635),#453,.T.);
#4998=ADVANCED_FACE('',(#636),#4775,.T.);
#4999=ADVANCED_FACE('',(#637),#4776,.T.);
#5000=ADVANCED_FACE('',(#638),#4777,.T.);
#5001=ADVANCED_FACE('',(#639),#454,.T.);
#5002=ADVANCED_FACE('',(#640),#4778,.T.);
#5003=ADVANCED_FACE('',(#641),#4779,.T.);
#5004=ADVANCED_FACE('',(#642),#4780,.T.);
#5005=ADVANCED_FACE('',(#643),#455,.T.);
#5006=ADVANCED_FACE('',(#644),#4781,.T.);
#5007=ADVANCED_FACE('',(#645),#4782,.T.);
#5008=ADVANCED_FACE('',(#646),#4783,.T.);
#5009=ADVANCED_FACE('',(#647),#4784,.T.);
#5010=ADVANCED_FACE('',(#648),#4785,.T.);
#5011=ADVANCED_FACE('',(#649),#4786,.T.);
#5012=ADVANCED_FACE('',(#650),#4787,.T.);
#5013=ADVANCED_FACE('',(#651),#4788,.T.);
#5014=ADVANCED_FACE('',(#652),#4789,.T.);
#5015=ADVANCED_FACE('',(#653),#4790,.T.);
#5016=ADVANCED_FACE('',(#654),#4791,.T.);
#5017=ADVANCED_FACE('',(#655),#456,.F.);
#5018=ADVANCED_FACE('',(#656,#114,#115,#116,#117,#118,#119,#120,#121,#122,
#123,#124,#125,#126,#127,#128,#129),#4792,.T.);
#5019=ADVANCED_FACE('',(#657,#130,#131,#132,#133,#134,#135,#136,#137,#138,
#139,#140,#141,#142,#143,#144,#145),#4793,.F.);
#5020=ADVANCED_FACE('',(#658),#457,.F.);
#5021=ADVANCED_FACE('',(#659),#4794,.F.);
#5022=ADVANCED_FACE('',(#660),#4795,.T.);
#5023=ADVANCED_FACE('',(#661),#4796,.T.);
#5024=ADVANCED_FACE('',(#662),#4797,.T.);
#5025=ADVANCED_FACE('',(#663,#146),#4798,.T.);
#5026=ADVANCED_FACE('',(#664,#147),#4799,.F.);
#5027=ADVANCED_FACE('',(#665),#4800,.T.);
#5028=ADVANCED_FACE('',(#666),#4801,.T.);
#5029=ADVANCED_FACE('',(#667),#458,.T.);
#5030=ADVANCED_FACE('',(#668),#4802,.T.);
#5031=ADVANCED_FACE('',(#669),#4803,.T.);
#5032=ADVANCED_FACE('',(#670),#459,.F.);
#5033=ADVANCED_FACE('',(#671),#4804,.T.);
#5034=ADVANCED_FACE('',(#672),#460,.T.);
#5035=ADVANCED_FACE('',(#673),#4805,.T.);
#5036=ADVANCED_FACE('',(#674),#461,.T.);
#5037=ADVANCED_FACE('',(#675,#148),#4806,.T.);
#5038=ADVANCED_FACE('',(#676,#149),#4807,.F.);
#5039=ADVANCED_FACE('',(#677),#462,.T.);
#5040=ADVANCED_FACE('',(#678),#4808,.F.);
#5041=ADVANCED_FACE('',(#679),#4809,.T.);
#5042=ADVANCED_FACE('',(#680,#150),#4810,.F.);
#5043=ADVANCED_FACE('',(#681),#4811,.F.);
#5044=ADVANCED_FACE('',(#682),#4812,.F.);
#5045=ADVANCED_FACE('',(#683),#4813,.F.);
#5046=ADVANCED_FACE('',(#684),#4814,.T.);
#5047=ADVANCED_FACE('',(#685),#55,.T.);
#5048=ADVANCED_FACE('',(#686),#4815,.T.);
#5049=ADVANCED_FACE('',(#687),#4816,.F.);
#5050=ADVANCED_FACE('',(#688),#463,.T.);
#5051=ADVANCED_FACE('',(#689),#464,.T.);
#5052=ADVANCED_FACE('',(#690),#4817,.T.);
#5053=ADVANCED_FACE('',(#691),#4818,.F.);
#5054=ADVANCED_FACE('',(#692),#465,.F.);
#5055=ADVANCED_FACE('',(#693),#466,.F.);
#5056=ADVANCED_FACE('',(#694),#467,.F.);
#5057=ADVANCED_FACE('',(#695),#43,.F.);
#5058=ADVANCED_FACE('',(#696),#56,.T.);
#5059=ADVANCED_FACE('',(#697),#468,.T.);
#5060=ADVANCED_FACE('',(#698),#57,.T.);
#5061=ADVANCED_FACE('',(#699),#44,.F.);
#5062=ADVANCED_FACE('',(#700,#151),#4819,.F.);
#5063=ADVANCED_FACE('',(#701,#152),#4820,.F.);
#5064=ADVANCED_FACE('',(#702,#153),#4821,.F.);
#5065=ADVANCED_FACE('',(#703,#154),#4822,.F.);
#5066=ADVANCED_FACE('',(#704),#45,.T.);
#5067=ADVANCED_FACE('',(#705),#469,.T.);
#5068=ADVANCED_FACE('',(#706),#58,.F.);
#5069=ADVANCED_FACE('',(#707),#470,.T.);
#5070=ADVANCED_FACE('',(#708),#59,.F.);
#5071=ADVANCED_FACE('',(#709),#471,.T.);
#5072=ADVANCED_FACE('',(#710),#46,.T.);
#5073=ADVANCED_FACE('',(#711),#60,.T.);
#5074=ADVANCED_FACE('',(#712),#472,.F.);
#5075=ADVANCED_FACE('',(#713),#61,.T.);
#5076=ADVANCED_FACE('',(#714,#155),#4823,.F.);
#5077=ADVANCED_FACE('',(#715,#156),#4824,.F.);
#5078=ADVANCED_FACE('',(#716,#157),#4825,.F.);
#5079=ADVANCED_FACE('',(#717,#158),#4826,.F.);
#5080=ADVANCED_FACE('',(#718),#473,.F.);
#5081=ADVANCED_FACE('',(#719),#62,.T.);
#5082=ADVANCED_FACE('',(#720),#47,.T.);
#5083=ADVANCED_FACE('',(#721),#63,.F.);
#5084=ADVANCED_FACE('',(#722),#64,.F.);
#5085=ADVANCED_FACE('',(#723),#48,.F.);
#5086=ADVANCED_FACE('',(#724),#65,.F.);
#5087=ADVANCED_FACE('',(#725),#66,.T.);
#5088=ADVANCED_FACE('',(#726),#49,.T.);
#5089=ADVANCED_FACE('',(#727),#67,.T.);
#5090=ADVANCED_FACE('',(#728),#68,.T.);
#5091=ADVANCED_FACE('',(#729),#50,.F.);
#5092=ADVANCED_FACE('',(#730,#159),#4827,.F.);
#5093=ADVANCED_FACE('',(#731,#160),#4828,.F.);
#5094=ADVANCED_FACE('',(#732,#161),#4829,.T.);
#5095=ADVANCED_FACE('',(#733,#162),#4830,.T.);
#5096=ADVANCED_FACE('',(#734,#163),#4831,.T.);
#5097=ADVANCED_FACE('',(#735),#474,.F.);
#5098=ADVANCED_FACE('',(#736),#69,.T.);
#5099=ADVANCED_FACE('',(#737),#51,.T.);
#5100=ADVANCED_FACE('',(#738),#70,.F.);
#5101=ADVANCED_FACE('',(#739),#71,.F.);
#5102=ADVANCED_FACE('',(#740),#52,.F.);
#5103=ADVANCED_FACE('',(#741),#72,.F.);
#5104=ADVANCED_FACE('',(#742),#73,.T.);
#5105=ADVANCED_FACE('',(#743),#53,.T.);
#5106=ADVANCED_FACE('',(#744),#74,.T.);
#5107=ADVANCED_FACE('',(#745),#75,.T.);
#5108=ADVANCED_FACE('',(#746),#54,.F.);
#5109=ADVANCED_FACE('',(#747,#164),#4832,.F.);
#5110=ADVANCED_FACE('',(#748,#165),#4833,.F.);
#5111=ADVANCED_FACE('',(#749,#166),#4834,.T.);
#5112=ADVANCED_FACE('',(#750,#167),#4835,.T.);
#5113=ADVANCED_FACE('',(#751,#168),#4836,.T.);
#5114=CLOSED_SHELL('',(#4837,#4838,#4839,#4840,#4841,#4842,#4843,#4844,
#4845,#4846,#4847,#4848,#4849,#4850,#4851,#4852,#4853,#4854,#4855,#4856,
#4857,#4858,#4859,#4860,#4861,#4862,#4863,#4864,#4865,#4866,#4867,#4868,
#4869,#4870,#4871,#4872,#4873,#4874,#4875,#4876,#4877,#4878,#4879,#4880,
#4881,#4882,#4883,#4884,#4885,#4886,#4887,#4888,#4889,#4890,#4891,#4892,
#4893,#4894,#4895,#4896,#4897,#4898,#4899,#4900,#4901,#4902,#4903,#4904,
#4905,#4906,#4907,#4908,#4909,#4910,#4911,#4912,#4913,#4914,#4915,#4916,
#4917,#4918,#4919,#4920,#4921,#4922,#4923,#4924,#4925,#4926,#4927,#4928,
#4929,#4930,#4931,#4932,#4933,#4934,#4935,#4936,#4937,#4938,#4939,#4940,
#4941,#4942,#4943,#4944,#4945,#4946,#4947,#4948,#4949,#4950,#4951,#4952,
#4953,#4954,#4955,#4956,#4957,#4958,#4959,#4960,#4961,#4962,#4963,#4964,
#4965,#4966,#4967,#4968,#4969,#4970,#4971,#4972,#4973,#4974,#4975,#4976,
#4977,#4978,#4979,#4980,#4981,#4982,#4983,#4984,#4985,#4986,#4987,#4988,
#4989,#4990,#4991,#4992,#4993,#4994,#4995,#4996,#4997,#4998,#4999,#5000,
#5001,#5002,#5003,#5004,#5005,#5006,#5007,#5008,#5009,#5010,#5011,#5012,
#5013,#5014,#5015,#5016,#5017,#5018,#5019));
#5115=CLOSED_SHELL('',(#5020,#5021,#5022,#5023,#5024,#5025,#5026));
#5116=CLOSED_SHELL('',(#5027,#5028,#5029,#5030,#5031,#5032,#5033,#5034,
#5035,#5036,#5037,#5038));
#5117=CLOSED_SHELL('',(#5039,#5040,#5041));
#5118=CLOSED_SHELL('',(#5042,#5043,#5044,#5045,#5046,#5047,#5048,#5049,
#5050));
#5119=CLOSED_SHELL('',(#5051,#5052,#5053));
#5120=CLOSED_SHELL('',(#5054,#5055,#5056,#5057,#5058,#5059,#5060,#5061,
#5062,#5063,#5064,#5065));
#5121=CLOSED_SHELL('',(#5066,#5067,#5068,#5069,#5070,#5071,#5072,#5073,
#5074,#5075,#5076,#5077,#5078,#5079));
#5122=CLOSED_SHELL('',(#5080,#5081,#5082,#5083,#5084,#5085,#5086,#5087,
#5088,#5089,#5090,#5091,#5092,#5093,#5094,#5095,#5096));
#5123=CLOSED_SHELL('',(#5097,#5098,#5099,#5100,#5101,#5102,#5103,#5104,
#5105,#5106,#5107,#5108,#5109,#5110,#5111,#5112,#5113));
#5124=DERIVED_UNIT_ELEMENT(#5138,1.);
#5125=DERIVED_UNIT_ELEMENT(#8781,-3.);
#5126=DERIVED_UNIT_ELEMENT(#5138,1.);
#5127=DERIVED_UNIT_ELEMENT(#8781,-3.);
#5128=DERIVED_UNIT_ELEMENT(#5138,1.);
#5129=DERIVED_UNIT_ELEMENT(#8781,-3.);
#5130=DERIVED_UNIT_ELEMENT(#5138,1.);
#5131=DERIVED_UNIT_ELEMENT(#8781,-3.);
#5132=DERIVED_UNIT_ELEMENT(#5138,1.);
#5133=DERIVED_UNIT_ELEMENT(#8781,-3.);
#5134=DERIVED_UNIT_ELEMENT(#5138,1.);
#5135=DERIVED_UNIT_ELEMENT(#8781,-3.);
#5136=DERIVED_UNIT_ELEMENT(#5138,1.);
#5137=DERIVED_UNIT_ELEMENT(#8781,-3.);
#5138=(
MASS_UNIT()
NAMED_UNIT(*)
SI_UNIT(.KILO.,.GRAM.)
);
#5139=DERIVED_UNIT((#5124,#5125));
#5140=DERIVED_UNIT((#5126,#5127));
#5141=DERIVED_UNIT((#5128,#5129));
#5142=DERIVED_UNIT((#5130,#5131));
#5143=DERIVED_UNIT((#5132,#5133));
#5144=DERIVED_UNIT((#5134,#5135));
#5145=DERIVED_UNIT((#5136,#5137));
#5146=MEASURE_REPRESENTATION_ITEM('density measure',
POSITIVE_RATIO_MEASURE(7850.),#5139);
#5147=MEASURE_REPRESENTATION_ITEM('density measure',
POSITIVE_RATIO_MEASURE(7850.),#5140);
#5148=MEASURE_REPRESENTATION_ITEM('density measure',
POSITIVE_RATIO_MEASURE(7850.),#5141);
#5149=MEASURE_REPRESENTATION_ITEM('density measure',
POSITIVE_RATIO_MEASURE(7850.),#5142);
#5150=MEASURE_REPRESENTATION_ITEM('density measure',
POSITIVE_RATIO_MEASURE(7850.),#5143);
#5151=MEASURE_REPRESENTATION_ITEM('density measure',
POSITIVE_RATIO_MEASURE(7850.),#5144);
#5152=MEASURE_REPRESENTATION_ITEM('density measure',
POSITIVE_RATIO_MEASURE(7850.),#5145);
#5153=PROPERTY_DEFINITION_REPRESENTATION(#5188,#5167);
#5154=PROPERTY_DEFINITION_REPRESENTATION(#5189,#5168);
#5155=PROPERTY_DEFINITION_REPRESENTATION(#5190,#5169);
#5156=PROPERTY_DEFINITION_REPRESENTATION(#5191,#5170);
#5157=PROPERTY_DEFINITION_REPRESENTATION(#5192,#5171);
#5158=PROPERTY_DEFINITION_REPRESENTATION(#5193,#5172);
#5159=PROPERTY_DEFINITION_REPRESENTATION(#5194,#5173);
#5160=PROPERTY_DEFINITION_REPRESENTATION(#5195,#5174);
#5161=PROPERTY_DEFINITION_REPRESENTATION(#5196,#5175);
#5162=PROPERTY_DEFINITION_REPRESENTATION(#5197,#5176);
#5163=PROPERTY_DEFINITION_REPRESENTATION(#5198,#5177);
#5164=PROPERTY_DEFINITION_REPRESENTATION(#5199,#5178);
#5165=PROPERTY_DEFINITION_REPRESENTATION(#5200,#5179);
#5166=PROPERTY_DEFINITION_REPRESENTATION(#5201,#5180);
#5167=REPRESENTATION('material name',(#5181),#8772);
#5168=REPRESENTATION('density',(#5146),#8772);
#5169=REPRESENTATION('material name',(#5182),#8773);
#5170=REPRESENTATION('density',(#5147),#8773);
#5171=REPRESENTATION('material name',(#5183),#8774);
#5172=REPRESENTATION('density',(#5148),#8774);
#5173=REPRESENTATION('material name',(#5184),#8775);
#5174=REPRESENTATION('density',(#5149),#8775);
#5175=REPRESENTATION('material name',(#5185),#8776);
#5176=REPRESENTATION('density',(#5150),#8776);
#5177=REPRESENTATION('material name',(#5186),#8777);
#5178=REPRESENTATION('density',(#5151),#8777);
#5179=REPRESENTATION('material name',(#5187),#8778);
#5180=REPRESENTATION('density',(#5152),#8778);
#5181=DESCRIPTIVE_REPRESENTATION_ITEM('Steel','Steel');
#5182=DESCRIPTIVE_REPRESENTATION_ITEM('Steel','Steel');
#5183=DESCRIPTIVE_REPRESENTATION_ITEM('Steel','Steel');
#5184=DESCRIPTIVE_REPRESENTATION_ITEM('Steel','Steel');
#5185=DESCRIPTIVE_REPRESENTATION_ITEM('Steel','Steel');
#5186=DESCRIPTIVE_REPRESENTATION_ITEM('Steel','Steel');
#5187=DESCRIPTIVE_REPRESENTATION_ITEM('Steel','Steel');
#5188=PROPERTY_DEFINITION('material property','material name',#8818);
#5189=PROPERTY_DEFINITION('material property','density of part',#8818);
#5190=PROPERTY_DEFINITION('material property','material name',#8819);
#5191=PROPERTY_DEFINITION('material property','density of part',#8819);
#5192=PROPERTY_DEFINITION('material property','material name',#8820);
#5193=PROPERTY_DEFINITION('material property','density of part',#8820);
#5194=PROPERTY_DEFINITION('material property','material name',#8821);
#5195=PROPERTY_DEFINITION('material property','density of part',#8821);
#5196=PROPERTY_DEFINITION('material property','material name',#8822);
#5197=PROPERTY_DEFINITION('material property','density of part',#8822);
#5198=PROPERTY_DEFINITION('material property','material name',#8823);
#5199=PROPERTY_DEFINITION('material property','density of part',#8823);
#5200=PROPERTY_DEFINITION('material property','material name',#8824);
#5201=PROPERTY_DEFINITION('material property','density of part',#8824);
#5202=AXIS2_PLACEMENT_3D('',#7247,#5722,#5723);
#5203=AXIS2_PLACEMENT_3D('',#7248,#5724,#5725);
#5204=AXIS2_PLACEMENT_3D('',#7249,#5726,#5727);
#5205=AXIS2_PLACEMENT_3D('',#7258,#5732,#5733);
#5206=AXIS2_PLACEMENT_3D('',#7264,#5737,#5738);
#5207=AXIS2_PLACEMENT_3D('',#7270,#5742,#5743);
#5208=AXIS2_PLACEMENT_3D('',#7272,#5744,#5745);
#5209=AXIS2_PLACEMENT_3D('',#7275,#5747,#5748);
#5210=AXIS2_PLACEMENT_3D('',#7276,#5749,#5750);
#5211=AXIS2_PLACEMENT_3D('',#7278,#5751,#5752);
#5212=AXIS2_PLACEMENT_3D('',#7281,#5754,#5755);
#5213=AXIS2_PLACEMENT_3D('',#7282,#5756,#5757);
#5214=AXIS2_PLACEMENT_3D('',#7291,#5762,#5763);
#5215=AXIS2_PLACEMENT_3D('',#7297,#5767,#5768);
#5216=AXIS2_PLACEMENT_3D('',#7303,#5772,#5773);
#5217=AXIS2_PLACEMENT_3D('',#7305,#5774,#5775);
#5218=AXIS2_PLACEMENT_3D('',#7308,#5777,#5778);
#5219=AXIS2_PLACEMENT_3D('',#7309,#5779,#5780);
#5220=AXIS2_PLACEMENT_3D('',#7311,#5781,#5782);
#5221=AXIS2_PLACEMENT_3D('',#7314,#5784,#5785);
#5222=AXIS2_PLACEMENT_3D('',#7315,#5786,#5787);
#5223=AXIS2_PLACEMENT_3D('',#7321,#5791,#5792);
#5224=AXIS2_PLACEMENT_3D('',#7327,#5796,#5797);
#5225=AXIS2_PLACEMENT_3D('',#7333,#5801,#5802);
#5226=AXIS2_PLACEMENT_3D('',#7335,#5803,#5804);
#5227=AXIS2_PLACEMENT_3D('',#7338,#5806,#5807);
#5228=AXIS2_PLACEMENT_3D('',#7339,#5808,#5809);
#5229=AXIS2_PLACEMENT_3D('',#7348,#5814,#5815);
#5230=AXIS2_PLACEMENT_3D('',#7354,#5819,#5820);
#5231=AXIS2_PLACEMENT_3D('',#7360,#5824,#5825);
#5232=AXIS2_PLACEMENT_3D('',#7362,#5826,#5827);
#5233=AXIS2_PLACEMENT_3D('',#7365,#5829,#5830);
#5234=AXIS2_PLACEMENT_3D('',#7366,#5831,#5832);
#5235=AXIS2_PLACEMENT_3D('',#7368,#5833,#5834);
#5236=AXIS2_PLACEMENT_3D('',#7371,#5836,#5837);
#5237=AXIS2_PLACEMENT_3D('',#7372,#5838,#5839);
#5238=AXIS2_PLACEMENT_3D('',#7378,#5843,#5844);
#5239=AXIS2_PLACEMENT_3D('',#7384,#5848,#5849);
#5240=AXIS2_PLACEMENT_3D('',#7387,#5852,#5853);
#5241=AXIS2_PLACEMENT_3D('',#7393,#5857,#5858);
#5242=AXIS2_PLACEMENT_3D('',#7399,#5862,#5863);
#5243=AXIS2_PLACEMENT_3D('',#7405,#5867,#5868);
#5244=AXIS2_PLACEMENT_3D('',#7407,#5869,#5870);
#5245=AXIS2_PLACEMENT_3D('',#7410,#5872,#5873);
#5246=AXIS2_PLACEMENT_3D('',#7411,#5874,#5875);
#5247=AXIS2_PLACEMENT_3D('',#7420,#5880,#5881);
#5248=AXIS2_PLACEMENT_3D('',#7426,#5885,#5886);
#5249=AXIS2_PLACEMENT_3D('',#7429,#5889,#5890);
#5250=AXIS2_PLACEMENT_3D('',#7431,#5891,#5892);
#5251=AXIS2_PLACEMENT_3D('',#7434,#5894,#5895);
#5252=AXIS2_PLACEMENT_3D('',#7435,#5896,#5897);
#5253=AXIS2_PLACEMENT_3D('',#7441,#5901,#5902);
#5254=AXIS2_PLACEMENT_3D('',#7447,#5906,#5907);
#5255=AXIS2_PLACEMENT_3D('',#7450,#5910,#5911);
#5256=AXIS2_PLACEMENT_3D('',#7459,#5916,#5917);
#5257=AXIS2_PLACEMENT_3D('',#7468,#5922,#5923);
#5258=AXIS2_PLACEMENT_3D('',#7470,#5924,#5925);
#5259=AXIS2_PLACEMENT_3D('',#7473,#5927,#5928);
#5260=AXIS2_PLACEMENT_3D('',#7474,#5929,#5930);
#5261=AXIS2_PLACEMENT_3D('',#7476,#5931,#5932);
#5262=AXIS2_PLACEMENT_3D('',#7479,#5934,#5935);
#5263=AXIS2_PLACEMENT_3D('',#7480,#5936,#5937);
#5264=AXIS2_PLACEMENT_3D('',#7482,#5938,#5939);
#5265=AXIS2_PLACEMENT_3D('',#7485,#5941,#5942);
#5266=AXIS2_PLACEMENT_3D('',#7486,#5943,#5944);
#5267=AXIS2_PLACEMENT_3D('',#7488,#5945,#5946);
#5268=AXIS2_PLACEMENT_3D('',#7491,#5948,#5949);
#5269=AXIS2_PLACEMENT_3D('',#7492,#5950,#5951);
#5270=AXIS2_PLACEMENT_3D('',#7495,#5954,#5955);
#5271=AXIS2_PLACEMENT_3D('',#7504,#5960,#5961);
#5272=AXIS2_PLACEMENT_3D('',#7506,#5962,#5963);
#5273=AXIS2_PLACEMENT_3D('',#7509,#5965,#5966);
#5274=AXIS2_PLACEMENT_3D('',#7510,#5967,#5968);
#5275=AXIS2_PLACEMENT_3D('',#7512,#5969,#5970);
#5276=AXIS2_PLACEMENT_3D('',#7515,#5972,#5973);
#5277=AXIS2_PLACEMENT_3D('',#7516,#5974,#5975);
#5278=AXIS2_PLACEMENT_3D('',#7525,#5980,#5981);
#5279=AXIS2_PLACEMENT_3D('',#7528,#5984,#5985);
#5280=AXIS2_PLACEMENT_3D('',#7530,#5986,#5987);
#5281=AXIS2_PLACEMENT_3D('',#7533,#5989,#5990);
#5282=AXIS2_PLACEMENT_3D('',#7534,#5991,#5992);
#5283=AXIS2_PLACEMENT_3D('',#7536,#5993,#5994);
#5284=AXIS2_PLACEMENT_3D('',#7539,#5996,#5997);
#5285=AXIS2_PLACEMENT_3D('',#7540,#5998,#5999);
#5286=AXIS2_PLACEMENT_3D('',#7549,#6004,#6005);
#5287=AXIS2_PLACEMENT_3D('',#7555,#6009,#6010);
#5288=AXIS2_PLACEMENT_3D('',#7561,#6014,#6015);
#5289=AXIS2_PLACEMENT_3D('',#7563,#6016,#6017);
#5290=AXIS2_PLACEMENT_3D('',#7566,#6019,#6020);
#5291=AXIS2_PLACEMENT_3D('',#7567,#6021,#6022);
#5292=AXIS2_PLACEMENT_3D('',#7569,#6023,#6024);
#5293=AXIS2_PLACEMENT_3D('',#7572,#6026,#6027);
#5294=AXIS2_PLACEMENT_3D('',#7573,#6028,#6029);
#5295=AXIS2_PLACEMENT_3D('',#7582,#6034,#6035);
#5296=AXIS2_PLACEMENT_3D('',#7588,#6039,#6040);
#5297=AXIS2_PLACEMENT_3D('',#7594,#6044,#6045);
#5298=AXIS2_PLACEMENT_3D('',#7596,#6046,#6047);
#5299=AXIS2_PLACEMENT_3D('',#7599,#6049,#6050);
#5300=AXIS2_PLACEMENT_3D('',#7600,#6051,#6052);
#5301=AXIS2_PLACEMENT_3D('',#7602,#6053,#6054);
#5302=AXIS2_PLACEMENT_3D('',#7605,#6056,#6057);
#5303=AXIS2_PLACEMENT_3D('',#7606,#6058,#6059);
#5304=AXIS2_PLACEMENT_3D('',#7612,#6063,#6064);
#5305=AXIS2_PLACEMENT_3D('',#7618,#6068,#6069);
#5306=AXIS2_PLACEMENT_3D('',#7624,#6073,#6074);
#5307=AXIS2_PLACEMENT_3D('',#7626,#6075,#6076);
#5308=AXIS2_PLACEMENT_3D('',#7629,#6078,#6079);
#5309=AXIS2_PLACEMENT_3D('',#7630,#6080,#6081);
#5310=AXIS2_PLACEMENT_3D('',#7636,#6085,#6086);
#5311=AXIS2_PLACEMENT_3D('',#7642,#6090,#6091);
#5312=AXIS2_PLACEMENT_3D('',#7645,#6094,#6095);
#5313=AXIS2_PLACEMENT_3D('',#7651,#6099,#6100);
#5314=AXIS2_PLACEMENT_3D('',#7657,#6104,#6105);
#5315=AXIS2_PLACEMENT_3D('',#7663,#6109,#6110);
#5316=AXIS2_PLACEMENT_3D('',#7665,#6111,#6112);
#5317=AXIS2_PLACEMENT_3D('',#7668,#6114,#6115);
#5318=AXIS2_PLACEMENT_3D('',#7669,#6116,#6117);
#5319=AXIS2_PLACEMENT_3D('',#7675,#6121,#6122);
#5320=AXIS2_PLACEMENT_3D('',#7681,#6126,#6127);
#5321=AXIS2_PLACEMENT_3D('',#7684,#6130,#6131);
#5322=AXIS2_PLACEMENT_3D('',#7693,#6136,#6137);
#5323=AXIS2_PLACEMENT_3D('',#7702,#6142,#6143);
#5324=AXIS2_PLACEMENT_3D('',#7704,#6144,#6145);
#5325=AXIS2_PLACEMENT_3D('',#7707,#6147,#6148);
#5326=AXIS2_PLACEMENT_3D('',#7708,#6149,#6150);
#5327=AXIS2_PLACEMENT_3D('',#7710,#6151,#6152);
#5328=AXIS2_PLACEMENT_3D('',#7713,#6154,#6155);
#5329=AXIS2_PLACEMENT_3D('',#7714,#6156,#6157);
#5330=AXIS2_PLACEMENT_3D('',#7716,#6158,#6159);
#5331=AXIS2_PLACEMENT_3D('',#7719,#6161,#6162);
#5332=AXIS2_PLACEMENT_3D('',#7720,#6163,#6164);
#5333=AXIS2_PLACEMENT_3D('',#7722,#6165,#6166);
#5334=AXIS2_PLACEMENT_3D('',#7725,#6168,#6169);
#5335=AXIS2_PLACEMENT_3D('',#7726,#6170,#6171);
#5336=AXIS2_PLACEMENT_3D('',#7729,#6174,#6175);
#5337=AXIS2_PLACEMENT_3D('',#7738,#6180,#6181);
#5338=AXIS2_PLACEMENT_3D('',#7740,#6182,#6183);
#5339=AXIS2_PLACEMENT_3D('',#7743,#6185,#6186);
#5340=AXIS2_PLACEMENT_3D('',#7744,#6187,#6188);
#5341=AXIS2_PLACEMENT_3D('',#7746,#6189,#6190);
#5342=AXIS2_PLACEMENT_3D('',#7749,#6192,#6193);
#5343=AXIS2_PLACEMENT_3D('',#7750,#6194,#6195);
#5344=AXIS2_PLACEMENT_3D('',#7759,#6200,#6201);
#5345=AXIS2_PLACEMENT_3D('',#7768,#6206,#6207);
#5346=AXIS2_PLACEMENT_3D('',#7770,#6208,#6209);
#5347=AXIS2_PLACEMENT_3D('',#7773,#6211,#6212);
#5348=AXIS2_PLACEMENT_3D('',#7774,#6213,#6214);
#5349=AXIS2_PLACEMENT_3D('',#7776,#6215,#6216);
#5350=AXIS2_PLACEMENT_3D('',#7779,#6218,#6219);
#5351=AXIS2_PLACEMENT_3D('',#7780,#6220,#6221);
#5352=AXIS2_PLACEMENT_3D('',#7782,#6222,#6223);
#5353=AXIS2_PLACEMENT_3D('',#7785,#6225,#6226);
#5354=AXIS2_PLACEMENT_3D('',#7786,#6227,#6228);
#5355=AXIS2_PLACEMENT_3D('',#7788,#6229,#6230);
#5356=AXIS2_PLACEMENT_3D('',#7791,#6232,#6233);
#5357=AXIS2_PLACEMENT_3D('',#7792,#6234,#6235);
#5358=AXIS2_PLACEMENT_3D('',#7801,#6240,#6241);
#5359=AXIS2_PLACEMENT_3D('',#7810,#6246,#6247);
#5360=AXIS2_PLACEMENT_3D('',#7812,#6248,#6249);
#5361=AXIS2_PLACEMENT_3D('',#7815,#6251,#6252);
#5362=AXIS2_PLACEMENT_3D('',#7816,#6253,#6254);
#5363=AXIS2_PLACEMENT_3D('',#7818,#6255,#6256);
#5364=AXIS2_PLACEMENT_3D('',#7821,#6258,#6259);
#5365=AXIS2_PLACEMENT_3D('',#7822,#6260,#6261);
#5366=AXIS2_PLACEMENT_3D('',#7824,#6262,#6263);
#5367=AXIS2_PLACEMENT_3D('',#7827,#6265,#6266);
#5368=AXIS2_PLACEMENT_3D('',#7828,#6267,#6268);
#5369=AXIS2_PLACEMENT_3D('',#7830,#6269,#6270);
#5370=AXIS2_PLACEMENT_3D('',#7833,#6272,#6273);
#5371=AXIS2_PLACEMENT_3D('',#7834,#6274,#6275);
#5372=AXIS2_PLACEMENT_3D('',#7837,#6278,#6279);
#5373=AXIS2_PLACEMENT_3D('',#7846,#6284,#6285);
#5374=AXIS2_PLACEMENT_3D('',#7848,#6286,#6287);
#5375=AXIS2_PLACEMENT_3D('',#7851,#6289,#6290);
#5376=AXIS2_PLACEMENT_3D('',#7852,#6291,#6292);
#5377=AXIS2_PLACEMENT_3D('',#7854,#6293,#6294);
#5378=AXIS2_PLACEMENT_3D('',#7857,#6296,#6297);
#5379=AXIS2_PLACEMENT_3D('',#7858,#6298,#6299);
#5380=AXIS2_PLACEMENT_3D('',#7861,#6302,#6303);
#5381=AXIS2_PLACEMENT_3D('',#7864,#6306,#6307);
#5382=AXIS2_PLACEMENT_3D('',#7867,#6310,#6311);
#5383=AXIS2_PLACEMENT_3D('',#7876,#6316,#6317);
#5384=AXIS2_PLACEMENT_3D('',#7878,#6318,#6319);
#5385=AXIS2_PLACEMENT_3D('',#7881,#6321,#6322);
#5386=AXIS2_PLACEMENT_3D('',#7882,#6323,#6324);
#5387=AXIS2_PLACEMENT_3D('',#7884,#6325,#6326);
#5388=AXIS2_PLACEMENT_3D('',#7887,#6328,#6329);
#5389=AXIS2_PLACEMENT_3D('',#7888,#6330,#6331);
#5390=AXIS2_PLACEMENT_3D('',#7891,#6334,#6335);
#5391=AXIS2_PLACEMENT_3D('',#7894,#6338,#6339);
#5392=AXIS2_PLACEMENT_3D('',#7903,#6344,#6345);
#5393=AXIS2_PLACEMENT_3D('',#7909,#6349,#6350);
#5394=AXIS2_PLACEMENT_3D('',#7915,#6354,#6355);
#5395=AXIS2_PLACEMENT_3D('',#7917,#6356,#6357);
#5396=AXIS2_PLACEMENT_3D('',#7920,#6359,#6360);
#5397=AXIS2_PLACEMENT_3D('',#7921,#6361,#6362);
#5398=AXIS2_PLACEMENT_3D('',#7923,#6363,#6364);
#5399=AXIS2_PLACEMENT_3D('',#7926,#6366,#6367);
#5400=AXIS2_PLACEMENT_3D('',#7927,#6368,#6369);
#5401=AXIS2_PLACEMENT_3D('',#7933,#6373,#6374);
#5402=AXIS2_PLACEMENT_3D('',#7939,#6378,#6379);
#5403=AXIS2_PLACEMENT_3D('',#7945,#6383,#6384);
#5404=AXIS2_PLACEMENT_3D('',#7947,#6385,#6386);
#5405=AXIS2_PLACEMENT_3D('',#7950,#6388,#6389);
#5406=AXIS2_PLACEMENT_3D('',#7951,#6390,#6391);
#5407=AXIS2_PLACEMENT_3D('',#7960,#6396,#6397);
#5408=AXIS2_PLACEMENT_3D('',#7966,#6401,#6402);
#5409=AXIS2_PLACEMENT_3D('',#7972,#6406,#6407);
#5410=AXIS2_PLACEMENT_3D('',#7974,#6408,#6409);
#5411=AXIS2_PLACEMENT_3D('',#7977,#6411,#6412);
#5412=AXIS2_PLACEMENT_3D('',#7978,#6413,#6414);
#5413=AXIS2_PLACEMENT_3D('',#7980,#6415,#6416);
#5414=AXIS2_PLACEMENT_3D('',#7983,#6418,#6419);
#5415=AXIS2_PLACEMENT_3D('',#7984,#6420,#6421);
#5416=AXIS2_PLACEMENT_3D('',#7993,#6426,#6427);
#5417=AXIS2_PLACEMENT_3D('',#7999,#6431,#6432);
#5418=AXIS2_PLACEMENT_3D('',#8005,#6436,#6437);
#5419=AXIS2_PLACEMENT_3D('',#8007,#6438,#6439);
#5420=AXIS2_PLACEMENT_3D('',#8010,#6441,#6442);
#5421=AXIS2_PLACEMENT_3D('',#8011,#6443,#6444);
#5422=AXIS2_PLACEMENT_3D('',#8013,#6445,#6446);
#5423=AXIS2_PLACEMENT_3D('',#8016,#6448,#6449);
#5424=AXIS2_PLACEMENT_3D('',#8017,#6450,#6451);
#5425=AXIS2_PLACEMENT_3D('',#8023,#6455,#6456);
#5426=AXIS2_PLACEMENT_3D('',#8029,#6460,#6461);
#5427=AXIS2_PLACEMENT_3D('',#8032,#6464,#6465);
#5428=AXIS2_PLACEMENT_3D('',#8038,#6469,#6470);
#5429=AXIS2_PLACEMENT_3D('',#8044,#6474,#6475);
#5430=AXIS2_PLACEMENT_3D('',#8047,#6478,#6479);
#5431=AXIS2_PLACEMENT_3D('',#8053,#6483,#6484);
#5432=AXIS2_PLACEMENT_3D('',#8059,#6488,#6489);
#5433=AXIS2_PLACEMENT_3D('',#8062,#6492,#6493);
#5434=AXIS2_PLACEMENT_3D('',#8068,#6497,#6498);
#5435=AXIS2_PLACEMENT_3D('',#8074,#6502,#6503);
#5436=AXIS2_PLACEMENT_3D('',#8080,#6507,#6508);
#5437=AXIS2_PLACEMENT_3D('',#8082,#6509,#6510);
#5438=AXIS2_PLACEMENT_3D('',#8085,#6512,#6513);
#5439=AXIS2_PLACEMENT_3D('',#8086,#6514,#6515);
#5440=AXIS2_PLACEMENT_3D('',#8089,#6518,#6519);
#5441=AXIS2_PLACEMENT_3D('',#8098,#6524,#6525);
#5442=AXIS2_PLACEMENT_3D('',#8100,#6526,#6527);
#5443=AXIS2_PLACEMENT_3D('',#8103,#6529,#6530);
#5444=AXIS2_PLACEMENT_3D('',#8104,#6531,#6532);
#5445=AXIS2_PLACEMENT_3D('',#8106,#6533,#6534);
#5446=AXIS2_PLACEMENT_3D('',#8109,#6536,#6537);
#5447=AXIS2_PLACEMENT_3D('',#8110,#6538,#6539);
#5448=AXIS2_PLACEMENT_3D('',#8119,#6544,#6545);
#5449=AXIS2_PLACEMENT_3D('',#8122,#6548,#6549);
#5450=AXIS2_PLACEMENT_3D('',#8124,#6550,#6551);
#5451=AXIS2_PLACEMENT_3D('',#8127,#6553,#6554);
#5452=AXIS2_PLACEMENT_3D('',#8128,#6555,#6556);
#5453=AXIS2_PLACEMENT_3D('',#8130,#6557,#6558);
#5454=AXIS2_PLACEMENT_3D('',#8133,#6560,#6561);
#5455=AXIS2_PLACEMENT_3D('',#8134,#6562,#6563);
#5456=AXIS2_PLACEMENT_3D('',#8137,#6566,#6567);
#5457=AXIS2_PLACEMENT_3D('',#8140,#6570,#6571);
#5458=AXIS2_PLACEMENT_3D('',#8149,#6576,#6577);
#5459=AXIS2_PLACEMENT_3D('',#8155,#6581,#6582);
#5460=AXIS2_PLACEMENT_3D('',#8161,#6586,#6587);
#5461=AXIS2_PLACEMENT_3D('',#8163,#6588,#6589);
#5462=AXIS2_PLACEMENT_3D('',#8166,#6591,#6592);
#5463=AXIS2_PLACEMENT_3D('',#8167,#6593,#6594);
#5464=AXIS2_PLACEMENT_3D('',#8169,#6595,#6596);
#5465=AXIS2_PLACEMENT_3D('',#8172,#6598,#6599);
#5466=AXIS2_PLACEMENT_3D('',#8173,#6600,#6601);
#5467=AXIS2_PLACEMENT_3D('',#8179,#6605,#6606);
#5468=AXIS2_PLACEMENT_3D('',#8185,#6610,#6611);
#5469=AXIS2_PLACEMENT_3D('',#8191,#6615,#6616);
#5470=AXIS2_PLACEMENT_3D('',#8193,#6617,#6618);
#5471=AXIS2_PLACEMENT_3D('',#8196,#6620,#6621);
#5472=AXIS2_PLACEMENT_3D('',#8197,#6622,#6623);
#5473=AXIS2_PLACEMENT_3D('',#8206,#6628,#6629);
#5474=AXIS2_PLACEMENT_3D('',#8212,#6633,#6634);
#5475=AXIS2_PLACEMENT_3D('',#8218,#6638,#6639);
#5476=AXIS2_PLACEMENT_3D('',#8220,#6640,#6641);
#5477=AXIS2_PLACEMENT_3D('',#8223,#6643,#6644);
#5478=AXIS2_PLACEMENT_3D('',#8224,#6645,#6646);
#5479=AXIS2_PLACEMENT_3D('',#8226,#6647,#6648);
#5480=AXIS2_PLACEMENT_3D('',#8229,#6650,#6651);
#5481=AXIS2_PLACEMENT_3D('',#8230,#6652,#6653);
#5482=AXIS2_PLACEMENT_3D('',#8236,#6657,#6658);
#5483=AXIS2_PLACEMENT_3D('',#8242,#6662,#6663);
#5484=AXIS2_PLACEMENT_3D('',#8248,#6667,#6668);
#5485=AXIS2_PLACEMENT_3D('',#8250,#6669,#6670);
#5486=AXIS2_PLACEMENT_3D('',#8253,#6672,#6673);
#5487=AXIS2_PLACEMENT_3D('',#8254,#6674,#6675);
#5488=AXIS2_PLACEMENT_3D('',#8260,#6679,#6680);
#5489=AXIS2_PLACEMENT_3D('',#8266,#6684,#6685);
#5490=AXIS2_PLACEMENT_3D('',#8272,#6689,#6690);
#5491=AXIS2_PLACEMENT_3D('',#8274,#6691,#6692);
#5492=AXIS2_PLACEMENT_3D('',#8277,#6694,#6695);
#5493=AXIS2_PLACEMENT_3D('',#8278,#6696,#6697);
#5494=AXIS2_PLACEMENT_3D('',#8284,#6701,#6702);
#5495=AXIS2_PLACEMENT_3D('',#8290,#6706,#6707);
#5496=AXIS2_PLACEMENT_3D('',#8293,#6710,#6711);
#5497=AXIS2_PLACEMENT_3D('',#8299,#6715,#6716);
#5498=AXIS2_PLACEMENT_3D('',#8305,#6720,#6721);
#5499=AXIS2_PLACEMENT_3D('',#8308,#6724,#6725);
#5500=AXIS2_PLACEMENT_3D('',#8314,#6729,#6730);
#5501=AXIS2_PLACEMENT_3D('',#8320,#6734,#6735);
#5502=AXIS2_PLACEMENT_3D('',#8323,#6738,#6739);
#5503=AXIS2_PLACEMENT_3D('',#8326,#6742,#6743);
#5504=AXIS2_PLACEMENT_3D('',#8329,#6746,#6747);
#5505=AXIS2_PLACEMENT_3D('',#8331,#6748,#6749);
#5506=AXIS2_PLACEMENT_3D('',#8334,#6751,#6752);
#5507=AXIS2_PLACEMENT_3D('',#8335,#6753,#6754);
#5508=AXIS2_PLACEMENT_3D('',#8336,#6755,#6756);
#5509=AXIS2_PLACEMENT_3D('',#8337,#6757,#6758);
#5510=AXIS2_PLACEMENT_3D('',#8338,#6759,#6760);
#5511=AXIS2_PLACEMENT_3D('',#8340,#6761,#6762);
#5512=AXIS2_PLACEMENT_3D('',#8343,#6764,#6765);
#5513=AXIS2_PLACEMENT_3D('',#8344,#6766,#6767);
#5514=AXIS2_PLACEMENT_3D('',#8353,#6772,#6773);
#5515=AXIS2_PLACEMENT_3D('',#8359,#6777,#6778);
#5516=AXIS2_PLACEMENT_3D('',#8365,#6782,#6783);
#5517=AXIS2_PLACEMENT_3D('',#8368,#6786,#6787);
#5518=AXIS2_PLACEMENT_3D('',#8369,#6788,#6789);
#5519=AXIS2_PLACEMENT_3D('',#8370,#6790,#6791);
#5520=AXIS2_PLACEMENT_3D('',#8371,#6792,#6793);
#5521=AXIS2_PLACEMENT_3D('',#8380,#6798,#6799);
#5522=AXIS2_PLACEMENT_3D('',#8389,#6804,#6805);
#5523=AXIS2_PLACEMENT_3D('',#8390,#6806,#6807);
#5524=AXIS2_PLACEMENT_3D('',#8391,#6808,#6809);
#5525=AXIS2_PLACEMENT_3D('',#8392,#6810,#6811);
#5526=AXIS2_PLACEMENT_3D('',#8401,#6816,#6817);
#5527=AXIS2_PLACEMENT_3D('',#8407,#6821,#6822);
#5528=AXIS2_PLACEMENT_3D('',#8409,#6823,#6824);
#5529=AXIS2_PLACEMENT_3D('',#8412,#6826,#6827);
#5530=AXIS2_PLACEMENT_3D('',#8413,#6828,#6829);
#5531=AXIS2_PLACEMENT_3D('',#8419,#6833,#6834);
#5532=AXIS2_PLACEMENT_3D('',#8420,#6835,#6836);
#5533=AXIS2_PLACEMENT_3D('',#8421,#6837,#6838);
#5534=AXIS2_PLACEMENT_3D('',#8422,#6839,#6840);
#5535=AXIS2_PLACEMENT_3D('',#8428,#6844,#6845);
#5536=AXIS2_PLACEMENT_3D('',#8429,#6846,#6847);
#5537=AXIS2_PLACEMENT_3D('',#8430,#6848,#6849);
#5538=AXIS2_PLACEMENT_3D('',#8431,#6850,#6851);
#5539=AXIS2_PLACEMENT_3D('',#8432,#6852,#6853);
#5540=AXIS2_PLACEMENT_3D('',#8433,#6854,#6855);
#5541=AXIS2_PLACEMENT_3D('',#8434,#6856,#6857);
#5542=AXIS2_PLACEMENT_3D('',#8436,#6858,#6859);
#5543=AXIS2_PLACEMENT_3D('',#8439,#6861,#6862);
#5544=AXIS2_PLACEMENT_3D('',#8440,#6863,#6864);
#5545=AXIS2_PLACEMENT_3D('',#8441,#6865,#6866);
#5546=AXIS2_PLACEMENT_3D('',#8442,#6867,#6868);
#5547=AXIS2_PLACEMENT_3D('',#8443,#6869,#6870);
#5548=AXIS2_PLACEMENT_3D('',#8445,#6871,#6872);
#5549=AXIS2_PLACEMENT_3D('',#8447,#6873,#6874);
#5550=AXIS2_PLACEMENT_3D('',#8448,#6875,#6876);
#5551=AXIS2_PLACEMENT_3D('',#8475,#6879,#6880);
#5552=AXIS2_PLACEMENT_3D('',#8478,#6881,#6882);
#5553=AXIS2_PLACEMENT_3D('',#8481,#6884,#6885);
#5554=AXIS2_PLACEMENT_3D('',#8482,#6886,#6887);
#5555=AXIS2_PLACEMENT_3D('',#8483,#6888,#6889);
#5556=AXIS2_PLACEMENT_3D('',#8507,#6891,#6892);
#5557=AXIS2_PLACEMENT_3D('',#8508,#6893,#6894);
#5558=AXIS2_PLACEMENT_3D('',#8509,#6895,#6896);
#5559=AXIS2_PLACEMENT_3D('',#8510,#6897,#6898);
#5560=AXIS2_PLACEMENT_3D('',#8511,#6899,#6900);
#5561=AXIS2_PLACEMENT_3D('',#8512,#6901,#6902);
#5562=AXIS2_PLACEMENT_3D('',#8513,#6903,#6904);
#5563=AXIS2_PLACEMENT_3D('',#8515,#6905,#6906);
#5564=AXIS2_PLACEMENT_3D('',#8516,#6907,#6908);
#5565=AXIS2_PLACEMENT_3D('',#8518,#6910,#6911);
#5566=AXIS2_PLACEMENT_3D('',#8519,#6912,#6913);
#5567=AXIS2_PLACEMENT_3D('',#8521,#6914,#6915);
#5568=AXIS2_PLACEMENT_3D('',#8524,#6917,#6918);
#5569=AXIS2_PLACEMENT_3D('',#8525,#6919,#6920);
#5570=AXIS2_PLACEMENT_3D('',#8526,#6921,#6922);
#5571=AXIS2_PLACEMENT_3D('',#8527,#6923,#6924);
#5572=AXIS2_PLACEMENT_3D('',#8528,#6925,#6926);
#5573=AXIS2_PLACEMENT_3D('',#8530,#6927,#6928);
#5574=AXIS2_PLACEMENT_3D('',#8533,#6930,#6931);
#5575=AXIS2_PLACEMENT_3D('',#8534,#6932,#6933);
#5576=AXIS2_PLACEMENT_3D('',#8536,#6934,#6935);
#5577=AXIS2_PLACEMENT_3D('',#8539,#6937,#6938);
#5578=AXIS2_PLACEMENT_3D('',#8540,#6939,#6940);
#5579=AXIS2_PLACEMENT_3D('',#8543,#6941,#6942);
#5580=AXIS2_PLACEMENT_3D('',#8544,#6943,#6944);
#5581=AXIS2_PLACEMENT_3D('',#8547,#6946,#6947);
#5582=AXIS2_PLACEMENT_3D('',#8548,#6948,#6949);
#5583=AXIS2_PLACEMENT_3D('',#8551,#6951,#6952);
#5584=AXIS2_PLACEMENT_3D('',#8552,#6953,#6954);
#5585=AXIS2_PLACEMENT_3D('',#8554,#6955,#6956);
#5586=AXIS2_PLACEMENT_3D('',#8556,#6957,#6958);
#5587=AXIS2_PLACEMENT_3D('',#8557,#6959,#6960);
#5588=AXIS2_PLACEMENT_3D('',#8558,#6961,#6962);
#5589=AXIS2_PLACEMENT_3D('',#8560,#6963,#6964);
#5590=AXIS2_PLACEMENT_3D('',#8562,#6966,#6967);
#5591=AXIS2_PLACEMENT_3D('',#8564,#6968,#6969);
#5592=AXIS2_PLACEMENT_3D('',#8565,#6970,#6971);
#5593=AXIS2_PLACEMENT_3D('',#8566,#6972,#6973);
#5594=AXIS2_PLACEMENT_3D('',#8569,#6975,#6976);
#5595=AXIS2_PLACEMENT_3D('',#8570,#6977,#6978);
#5596=AXIS2_PLACEMENT_3D('',#8571,#6979,#6980);
#5597=AXIS2_PLACEMENT_3D('',#8572,#6981,#6982);
#5598=AXIS2_PLACEMENT_3D('',#8573,#6983,#6984);
#5599=AXIS2_PLACEMENT_3D('',#8574,#6985,#6986);
#5600=AXIS2_PLACEMENT_3D('',#8577,#6987,#6988);
#5601=AXIS2_PLACEMENT_3D('',#8580,#6990,#6991);
#5602=AXIS2_PLACEMENT_3D('',#8581,#6992,#6993);
#5603=AXIS2_PLACEMENT_3D('',#8582,#6994,#6995);
#5604=AXIS2_PLACEMENT_3D('',#8585,#6997,#6998);
#5605=AXIS2_PLACEMENT_3D('',#8586,#6999,#7000);
#5606=AXIS2_PLACEMENT_3D('',#8588,#7001,#7002);
#5607=AXIS2_PLACEMENT_3D('',#8589,#7003,#7004);
#5608=AXIS2_PLACEMENT_3D('',#8590,#7005,#7006);
#5609=AXIS2_PLACEMENT_3D('',#8592,#7007,#7008);
#5610=AXIS2_PLACEMENT_3D('',#8595,#7010,#7011);
#5611=AXIS2_PLACEMENT_3D('',#8596,#7012,#7013);
#5612=AXIS2_PLACEMENT_3D('',#8598,#7014,#7015);
#5613=AXIS2_PLACEMENT_3D('',#8600,#7016,#7017);
#5614=AXIS2_PLACEMENT_3D('',#8601,#7018,#7019);
#5615=AXIS2_PLACEMENT_3D('',#8602,#7020,#7021);
#5616=AXIS2_PLACEMENT_3D('',#8605,#7023,#7024);
#5617=AXIS2_PLACEMENT_3D('',#8606,#7025,#7026);
#5618=AXIS2_PLACEMENT_3D('',#8609,#7028,#7029);
#5619=AXIS2_PLACEMENT_3D('',#8610,#7030,#7031);
#5620=AXIS2_PLACEMENT_3D('',#8612,#7032,#7033);
#5621=AXIS2_PLACEMENT_3D('',#8614,#7034,#7035);
#5622=AXIS2_PLACEMENT_3D('',#8615,#7036,#7037);
#5623=AXIS2_PLACEMENT_3D('',#8616,#7038,#7039);
#5624=AXIS2_PLACEMENT_3D('',#8619,#7041,#7042);
#5625=AXIS2_PLACEMENT_3D('',#8620,#7043,#7044);
#5626=AXIS2_PLACEMENT_3D('',#8622,#7045,#7046);
#5627=AXIS2_PLACEMENT_3D('',#8623,#7047,#7048);
#5628=AXIS2_PLACEMENT_3D('',#8624,#7049,#7050);
#5629=AXIS2_PLACEMENT_3D('',#8625,#7051,#7052);
#5630=AXIS2_PLACEMENT_3D('',#8626,#7053,#7054);
#5631=AXIS2_PLACEMENT_3D('',#8627,#7055,#7056);
#5632=AXIS2_PLACEMENT_3D('',#8628,#7057,#7058);
#5633=AXIS2_PLACEMENT_3D('',#8630,#7059,#7060);
#5634=AXIS2_PLACEMENT_3D('',#8633,#7062,#7063);
#5635=AXIS2_PLACEMENT_3D('',#8634,#7064,#7065);
#5636=AXIS2_PLACEMENT_3D('',#8636,#7066,#7067);
#5637=AXIS2_PLACEMENT_3D('',#8638,#7068,#7069);
#5638=AXIS2_PLACEMENT_3D('',#8639,#7070,#7071);
#5639=AXIS2_PLACEMENT_3D('',#8640,#7072,#7073);
#5640=AXIS2_PLACEMENT_3D('',#8642,#7074,#7075);
#5641=AXIS2_PLACEMENT_3D('',#8644,#7077,#7078);
#5642=AXIS2_PLACEMENT_3D('',#8646,#7079,#7080);
#5643=AXIS2_PLACEMENT_3D('',#8647,#7081,#7082);
#5644=AXIS2_PLACEMENT_3D('',#8648,#7083,#7084);
#5645=AXIS2_PLACEMENT_3D('',#8650,#7085,#7086);
#5646=AXIS2_PLACEMENT_3D('',#8652,#7087,#7088);
#5647=AXIS2_PLACEMENT_3D('',#8653,#7089,#7090);
#5648=AXIS2_PLACEMENT_3D('',#8654,#7091,#7092);
#5649=AXIS2_PLACEMENT_3D('',#8656,#7093,#7094);
#5650=AXIS2_PLACEMENT_3D('',#8658,#7096,#7097);
#5651=AXIS2_PLACEMENT_3D('',#8660,#7098,#7099);
#5652=AXIS2_PLACEMENT_3D('',#8661,#7100,#7101);
#5653=AXIS2_PLACEMENT_3D('',#8662,#7102,#7103);
#5654=AXIS2_PLACEMENT_3D('',#8664,#7104,#7105);
#5655=AXIS2_PLACEMENT_3D('',#8666,#7106,#7107);
#5656=AXIS2_PLACEMENT_3D('',#8667,#7108,#7109);
#5657=AXIS2_PLACEMENT_3D('',#8668,#7110,#7111);
#5658=AXIS2_PLACEMENT_3D('',#8670,#7112,#7113);
#5659=AXIS2_PLACEMENT_3D('',#8672,#7115,#7116);
#5660=AXIS2_PLACEMENT_3D('',#8674,#7117,#7118);
#5661=AXIS2_PLACEMENT_3D('',#8675,#7119,#7120);
#5662=AXIS2_PLACEMENT_3D('',#8676,#7121,#7122);
#5663=AXIS2_PLACEMENT_3D('',#8678,#7123,#7124);
#5664=AXIS2_PLACEMENT_3D('',#8680,#7125,#7126);
#5665=AXIS2_PLACEMENT_3D('',#8681,#7127,#7128);
#5666=AXIS2_PLACEMENT_3D('',#8682,#7129,#7130);
#5667=AXIS2_PLACEMENT_3D('',#8684,#7131,#7132);
#5668=AXIS2_PLACEMENT_3D('',#8686,#7134,#7135);
#5669=AXIS2_PLACEMENT_3D('',#8687,#7136,#7137);
#5670=AXIS2_PLACEMENT_3D('',#8688,#7138,#7139);
#5671=AXIS2_PLACEMENT_3D('',#8689,#7140,#7141);
#5672=AXIS2_PLACEMENT_3D('',#8690,#7142,#7143);
#5673=AXIS2_PLACEMENT_3D('',#8691,#7144,#7145);
#5674=AXIS2_PLACEMENT_3D('',#8693,#7146,#7147);
#5675=AXIS2_PLACEMENT_3D('',#8696,#7149,#7150);
#5676=AXIS2_PLACEMENT_3D('',#8697,#7151,#7152);
#5677=AXIS2_PLACEMENT_3D('',#8699,#7153,#7154);
#5678=AXIS2_PLACEMENT_3D('',#8701,#7155,#7156);
#5679=AXIS2_PLACEMENT_3D('',#8702,#7157,#7158);
#5680=AXIS2_PLACEMENT_3D('',#8703,#7159,#7160);
#5681=AXIS2_PLACEMENT_3D('',#8705,#7161,#7162);
#5682=AXIS2_PLACEMENT_3D('',#8707,#7164,#7165);
#5683=AXIS2_PLACEMENT_3D('',#8709,#7166,#7167);
#5684=AXIS2_PLACEMENT_3D('',#8710,#7168,#7169);
#5685=AXIS2_PLACEMENT_3D('',#8711,#7170,#7171);
#5686=AXIS2_PLACEMENT_3D('',#8713,#7172,#7173);
#5687=AXIS2_PLACEMENT_3D('',#8715,#7174,#7175);
#5688=AXIS2_PLACEMENT_3D('',#8716,#7176,#7177);
#5689=AXIS2_PLACEMENT_3D('',#8717,#7178,#7179);
#5690=AXIS2_PLACEMENT_3D('',#8719,#7180,#7181);
#5691=AXIS2_PLACEMENT_3D('',#8721,#7183,#7184);
#5692=AXIS2_PLACEMENT_3D('',#8723,#7185,#7186);
#5693=AXIS2_PLACEMENT_3D('',#8724,#7187,#7188);
#5694=AXIS2_PLACEMENT_3D('',#8725,#7189,#7190);
#5695=AXIS2_PLACEMENT_3D('',#8727,#7191,#7192);
#5696=AXIS2_PLACEMENT_3D('',#8729,#7193,#7194);
#5697=AXIS2_PLACEMENT_3D('',#8730,#7195,#7196);
#5698=AXIS2_PLACEMENT_3D('',#8731,#7197,#7198);
#5699=AXIS2_PLACEMENT_3D('',#8733,#7199,#7200);
#5700=AXIS2_PLACEMENT_3D('',#8735,#7202,#7203);
#5701=AXIS2_PLACEMENT_3D('',#8737,#7204,#7205);
#5702=AXIS2_PLACEMENT_3D('',#8738,#7206,#7207);
#5703=AXIS2_PLACEMENT_3D('',#8739,#7208,#7209);
#5704=AXIS2_PLACEMENT_3D('',#8741,#7210,#7211);
#5705=AXIS2_PLACEMENT_3D('',#8743,#7212,#7213);
#5706=AXIS2_PLACEMENT_3D('',#8744,#7214,#7215);
#5707=AXIS2_PLACEMENT_3D('',#8745,#7216,#7217);
#5708=AXIS2_PLACEMENT_3D('',#8747,#7218,#7219);
#5709=AXIS2_PLACEMENT_3D('',#8749,#7221,#7222);
#5710=AXIS2_PLACEMENT_3D('',#8750,#7223,#7224);
#5711=AXIS2_PLACEMENT_3D('',#8751,#7225,#7226);
#5712=AXIS2_PLACEMENT_3D('',#8752,#7227,#7228);
#5713=AXIS2_PLACEMENT_3D('',#8753,#7229,#7230);
#5714=AXIS2_PLACEMENT_3D('',#8754,#7231,#7232);
#5715=AXIS2_PLACEMENT_3D('',#8755,#7233,#7234);
#5716=AXIS2_PLACEMENT_3D('',#8756,#7235,#7236);
#5717=AXIS2_PLACEMENT_3D('',#8757,#7237,#7238);
#5718=AXIS2_PLACEMENT_3D('',#8758,#7239,#7240);
#5719=AXIS2_PLACEMENT_3D('',#8759,#7241,#7242);
#5720=AXIS2_PLACEMENT_3D('',#8760,#7243,#7244);
#5721=AXIS2_PLACEMENT_3D('',#8761,#7245,#7246);
#5722=DIRECTION('axis',(0.,0.,1.));
#5723=DIRECTION('refdir',(1.,0.,0.));
#5724=DIRECTION('axis',(0.,0.,1.));
#5725=DIRECTION('refdir',(1.,0.,0.));
#5726=DIRECTION('center_axis',(-0.169919004238536,0.,0.985458031576477));
#5727=DIRECTION('ref_axis',(-0.985458031576477,0.,-0.169919004238536));
#5728=DIRECTION('',(0.985458031576477,0.,0.169919004238536));
#5729=DIRECTION('',(0.,1.,0.));
#5730=DIRECTION('',(-0.985458031576477,0.,-0.169919004238536));
#5731=DIRECTION('',(0.,-1.,0.));
#5732=DIRECTION('center_axis',(0.947303919134588,0.,0.320336205871659));
#5733=DIRECTION('ref_axis',(-0.320336205871659,0.,0.947303919134588));
#5734=DIRECTION('',(0.320336205871659,0.,-0.947303919134588));
#5735=DIRECTION('',(-0.320336205871659,0.,0.947303919134588));
#5736=DIRECTION('',(0.,-1.,0.));
#5737=DIRECTION('center_axis',(0.474184356164994,0.,-0.880425576848146));
#5738=DIRECTION('ref_axis',(0.880425576848146,0.,0.474184356164994));
#5739=DIRECTION('',(-0.880425576848146,0.,-0.474184356164994));
#5740=DIRECTION('',(0.880425576848146,0.,0.474184356164994));
#5741=DIRECTION('',(0.,-1.,0.));
#5742=DIRECTION('center_axis',(0.,-1.,0.));
#5743=DIRECTION('ref_axis',(1.,0.,0.));
#5744=DIRECTION('center_axis',(0.,1.,0.));
#5745=DIRECTION('ref_axis',(1.,0.,0.));
#5746=DIRECTION('',(0.,-1.,0.));
#5747=DIRECTION('center_axis',(0.,-1.,0.));
#5748=DIRECTION('ref_axis',(1.,0.,0.));
#5749=DIRECTION('center_axis',(0.,-1.,0.));
#5750=DIRECTION('ref_axis',(1.,0.,0.));
#5751=DIRECTION('center_axis',(0.,-1.,0.));
#5752=DIRECTION('ref_axis',(1.,0.,0.));
#5753=DIRECTION('',(0.,1.,0.));
#5754=DIRECTION('center_axis',(0.,1.,0.));
#5755=DIRECTION('ref_axis',(1.,0.,0.));
#5756=DIRECTION('center_axis',(0.441770335617579,0.,0.897128179564287));
#5757=DIRECTION('ref_axis',(-0.897128179564287,0.,0.441770335617579));
#5758=DIRECTION('',(0.897128179564287,0.,-0.441770335617579));
#5759=DIRECTION('',(0.,1.,0.));
#5760=DIRECTION('',(-0.897128179564287,0.,0.441770335617579));
#5761=DIRECTION('',(0.,-1.,0.));
#5762=DIRECTION('center_axis',(0.95467386700456,0.,-0.297653838642408));
#5763=DIRECTION('ref_axis',(0.297653838642408,0.,0.95467386700456));
#5764=DIRECTION('',(-0.297653838642408,0.,-0.95467386700456));
#5765=DIRECTION('',(0.297653838642408,0.,0.95467386700456));
#5766=DIRECTION('',(0.,-1.,0.));
#5767=DIRECTION('center_axis',(-0.13387796720821,0.,-0.990997825374101));
#5768=DIRECTION('ref_axis',(0.990997825374101,0.,-0.13387796720821));
#5769=DIRECTION('',(-0.990997825374101,0.,0.13387796720821));
#5770=DIRECTION('',(0.990997825374101,0.,-0.13387796720821));
#5771=DIRECTION('',(0.,-1.,0.));
#5772=DIRECTION('center_axis',(0.,-1.,0.));
#5773=DIRECTION('ref_axis',(1.,0.,0.));
#5774=DIRECTION('center_axis',(0.,1.,0.));
#5775=DIRECTION('ref_axis',(1.,0.,0.));
#5776=DIRECTION('',(0.,-1.,0.));
#5777=DIRECTION('center_axis',(0.,-1.,0.));
#5778=DIRECTION('ref_axis',(1.,0.,0.));
#5779=DIRECTION('center_axis',(0.,-1.,0.));
#5780=DIRECTION('ref_axis',(1.,0.,0.));
#5781=DIRECTION('center_axis',(0.,-1.,0.));
#5782=DIRECTION('ref_axis',(1.,0.,0.));
#5783=DIRECTION('',(0.,1.,0.));
#5784=DIRECTION('center_axis',(0.,1.,0.));
#5785=DIRECTION('ref_axis',(1.,0.,0.));
#5786=DIRECTION('center_axis',(0.0386823792600046,0.,0.999251556683694));
#5787=DIRECTION('ref_axis',(-0.999251556683694,0.,0.0386823792600046));
#5788=DIRECTION('',(0.999251556683694,0.,-0.0386823792600046));
#5789=DIRECTION('',(-0.999251556683694,0.,0.0386823792600046));
#5790=DIRECTION('',(0.,-1.,0.));
#5791=DIRECTION('center_axis',(0.993204697860151,0.,0.116380531655973));
#5792=DIRECTION('ref_axis',(-0.116380531655973,0.,0.993204697860151));
#5793=DIRECTION('',(0.116380531655973,0.,-0.993204697860151));
#5794=DIRECTION('',(-0.116380531655973,0.,0.993204697860151));
#5795=DIRECTION('',(0.,-1.,0.));
#5796=DIRECTION('center_axis',(0.280771519966595,0.,-0.959774636868285));
#5797=DIRECTION('ref_axis',(0.959774636868285,0.,0.280771519966595));
#5798=DIRECTION('',(-0.959774636868285,0.,-0.280771519966595));
#5799=DIRECTION('',(0.959774636868285,0.,0.280771519966595));
#5800=DIRECTION('',(0.,-1.,0.));
#5801=DIRECTION('center_axis',(0.,-1.,0.));
#5802=DIRECTION('ref_axis',(1.,0.,0.));
#5803=DIRECTION('center_axis',(0.,-1.,0.));
#5804=DIRECTION('ref_axis',(1.,0.,0.));
#5805=DIRECTION('',(0.,1.,0.));
#5806=DIRECTION('center_axis',(0.,1.,0.));
#5807=DIRECTION('ref_axis',(1.,0.,0.));
#5808=DIRECTION('center_axis',(0.884718422489227,0.,0.466125855223859));
#5809=DIRECTION('ref_axis',(-0.466125855223859,0.,0.884718422489227));
#5810=DIRECTION('',(0.466125855223858,0.,-0.884718422489227));
#5811=DIRECTION('',(0.,1.,0.));
#5812=DIRECTION('',(-0.466125855223858,0.,0.884718422489227));
#5813=DIRECTION('',(0.,-1.,0.));
#5814=DIRECTION('center_axis',(0.597390845850087,0.,-0.801950233676952));
#5815=DIRECTION('ref_axis',(0.801950233676952,0.,0.597390845850087));
#5816=DIRECTION('',(-0.801950233676952,0.,-0.597390845850087));
#5817=DIRECTION('',(0.801950233676952,0.,0.597390845850087));
#5818=DIRECTION('',(0.,-1.,0.));
#5819=DIRECTION('center_axis',(-0.690803457452622,0.,-0.723042587384383));
#5820=DIRECTION('ref_axis',(0.723042587384383,0.,-0.690803457452622));
#5821=DIRECTION('',(-0.723042587384383,0.,0.690803457452622));
#5822=DIRECTION('',(0.723042587384383,0.,-0.690803457452622));
#5823=DIRECTION('',(0.,-1.,0.));
#5824=DIRECTION('center_axis',(0.,-1.,0.));
#5825=DIRECTION('ref_axis',(1.,0.,0.));
#5826=DIRECTION('center_axis',(0.,1.,0.));
#5827=DIRECTION('ref_axis',(1.,0.,0.));
#5828=DIRECTION('',(0.,-1.,0.));
#5829=DIRECTION('center_axis',(0.,-1.,0.));
#5830=DIRECTION('ref_axis',(1.,0.,0.));
#5831=DIRECTION('center_axis',(0.,-1.,0.));
#5832=DIRECTION('ref_axis',(1.,0.,0.));
#5833=DIRECTION('center_axis',(0.,-1.,0.));
#5834=DIRECTION('ref_axis',(1.,0.,0.));
#5835=DIRECTION('',(0.,1.,0.));
#5836=DIRECTION('center_axis',(0.,1.,0.));
#5837=DIRECTION('ref_axis',(1.,0.,0.));
#5838=DIRECTION('center_axis',(0.245593157166234,0.,0.969372993822874));
#5839=DIRECTION('ref_axis',(-0.969372993822874,0.,0.245593157166234));
#5840=DIRECTION('',(0.969372993822874,0.,-0.245593157166234));
#5841=DIRECTION('',(-0.969372993822874,0.,0.245593157166234));
#5842=DIRECTION('',(0.,-1.,0.));
#5843=DIRECTION('center_axis',(0.995697665364314,0.,-0.0926615302488318));
#5844=DIRECTION('ref_axis',(0.0926615302488318,0.,0.995697665364314));
#5845=DIRECTION('',(-0.0926615302488317,0.,-0.995697665364314));
#5846=DIRECTION('',(0.0926615302488317,0.,0.995697665364314));
#5847=DIRECTION('',(0.,-1.,0.));
#5848=DIRECTION('center_axis',(0.075087621054422,0.,-0.997176939747599));
#5849=DIRECTION('ref_axis',(0.997176939747599,0.,0.075087621054422));
#5850=DIRECTION('',(-0.997176939747599,0.,-0.075087621054422));
#5851=DIRECTION('',(0.997176939747599,0.,0.075087621054422));
#5852=DIRECTION('center_axis',(0.618640030553172,0.,0.785674558960115));
#5853=DIRECTION('ref_axis',(-0.785674558960115,0.,0.618640030553172));
#5854=DIRECTION('',(0.785674558960114,0.,-0.618640030553172));
#5855=DIRECTION('',(-0.785674558960115,0.,0.618640030553172));
#5856=DIRECTION('',(0.,-1.,0.));
#5857=DIRECTION('center_axis',(0.871926239623235,0.,-0.489637245985725));
#5858=DIRECTION('ref_axis',(0.489637245985725,0.,0.871926239623235));
#5859=DIRECTION('',(-0.489637245985725,0.,-0.871926239623235));
#5860=DIRECTION('',(0.489637245985725,0.,0.871926239623235));
#5861=DIRECTION('',(0.,-1.,0.));
#5862=DIRECTION('center_axis',(-0.336992445886082,0.,-0.941507350696592));
#5863=DIRECTION('ref_axis',(0.941507350696592,0.,-0.336992445886082));
#5864=DIRECTION('',(-0.941507350696592,0.,0.336992445886082));
#5865=DIRECTION('',(0.941507350696592,0.,-0.336992445886082));
#5866=DIRECTION('',(0.,-1.,0.));
#5867=DIRECTION('center_axis',(0.,-1.,0.));
#5868=DIRECTION('ref_axis',(1.,0.,0.));
#5869=DIRECTION('center_axis',(0.,-1.,0.));
#5870=DIRECTION('ref_axis',(1.,0.,0.));
#5871=DIRECTION('',(0.,1.,0.));
#5872=DIRECTION('center_axis',(0.,1.,0.));
#5873=DIRECTION('ref_axis',(1.,0.,0.));
#5874=DIRECTION('center_axis',(-0.371094111890007,0.,0.928595261737086));
#5875=DIRECTION('ref_axis',(-0.928595261737086,0.,-0.371094111890007));
#5876=DIRECTION('',(0.928595261737086,0.,0.371094111890007));
#5877=DIRECTION('',(0.,1.,0.));
#5878=DIRECTION('',(-0.928595261737086,0.,-0.371094111890007));
#5879=DIRECTION('',(0.,-1.,0.));
#5880=DIRECTION('center_axis',(0.860001413474306,0.,0.510291650747096));
#5881=DIRECTION('ref_axis',(-0.510291650747096,0.,0.860001413474306));
#5882=DIRECTION('',(0.510291650747096,0.,-0.860001413474306));
#5883=DIRECTION('',(-0.510291650747096,0.,0.860001413474306));
#5884=DIRECTION('',(0.,-1.,0.));
#5885=DIRECTION('center_axis',(0.646873060609993,0.,-0.762597694369096));
#5886=DIRECTION('ref_axis',(0.762597694369096,0.,0.646873060609993));
#5887=DIRECTION('',(-0.762597694369096,0.,-0.646873060609993));
#5888=DIRECTION('',(0.762597694369096,0.,0.646873060609993));
#5889=DIRECTION('center_axis',(0.,-1.,0.));
#5890=DIRECTION('ref_axis',(1.,0.,0.));
#5891=DIRECTION('center_axis',(0.,1.,0.));
#5892=DIRECTION('ref_axis',(1.,0.,0.));
#5893=DIRECTION('',(0.,-1.,0.));
#5894=DIRECTION('center_axis',(0.,-1.,0.));
#5895=DIRECTION('ref_axis',(1.,0.,0.));
#5896=DIRECTION('center_axis',(0.768472187589369,0.,0.639883190044566));
#5897=DIRECTION('ref_axis',(-0.639883190044566,0.,0.768472187589369));
#5898=DIRECTION('',(0.639883190044566,0.,-0.768472187589369));
#5899=DIRECTION('',(-0.639883190044566,0.,0.768472187589368));
#5900=DIRECTION('',(0.,-1.,0.));
#5901=DIRECTION('center_axis',(0.751071251604073,0.,-0.660221156139283));
#5902=DIRECTION('ref_axis',(0.660221156139283,0.,0.751071251604073));
#5903=DIRECTION('',(-0.660221156139283,0.,-0.751071251604073));
#5904=DIRECTION('',(0.660221156139283,0.,0.751071251604073));
#5905=DIRECTION('',(0.,-1.,0.));
#5906=DIRECTION('center_axis',(-0.525378737609566,0.,-0.850868486940126));
#5907=DIRECTION('ref_axis',(0.850868486940126,0.,-0.525378737609566));
#5908=DIRECTION('',(-0.850868486940126,0.,0.525378737609565));
#5909=DIRECTION('',(0.850868486940126,0.,-0.525378737609565));
#5910=DIRECTION('center_axis',(-0.743144825477394,0.,-0.669130606358858));
#5911=DIRECTION('ref_axis',(0.669130606358858,0.,-0.743144825477394));
#5912=DIRECTION('',(-0.669130606358858,0.,0.743144825477394));
#5913=DIRECTION('',(0.,1.,0.));
#5914=DIRECTION('',(0.669130606358858,0.,-0.743144825477394));
#5915=DIRECTION('',(0.,-1.,0.));
#5916=DIRECTION('center_axis',(0.743144825477394,0.,0.669130606358858));
#5917=DIRECTION('ref_axis',(-0.669130606358858,0.,0.743144825477394));
#5918=DIRECTION('',(0.669130606358858,0.,-0.743144825477394));
#5919=DIRECTION('',(0.,1.,0.));
#5920=DIRECTION('',(-0.669130606358858,0.,0.743144825477394));
#5921=DIRECTION('',(0.,-1.,0.));
#5922=DIRECTION('center_axis',(0.,-1.,0.));
#5923=DIRECTION('ref_axis',(1.,0.,0.));
#5924=DIRECTION('center_axis',(0.,-1.,0.));
#5925=DIRECTION('ref_axis',(1.,0.,0.));
#5926=DIRECTION('',(0.,-1.,0.));
#5927=DIRECTION('center_axis',(0.,1.,0.));
#5928=DIRECTION('ref_axis',(1.,0.,0.));
#5929=DIRECTION('center_axis',(0.,-1.,0.));
#5930=DIRECTION('ref_axis',(1.,0.,0.));
#5931=DIRECTION('center_axis',(0.,1.,0.));
#5932=DIRECTION('ref_axis',(1.,0.,0.));
#5933=DIRECTION('',(0.,1.,0.));
#5934=DIRECTION('center_axis',(0.,-1.,0.));
#5935=DIRECTION('ref_axis',(1.,0.,0.));
#5936=DIRECTION('center_axis',(0.,-1.,0.));
#5937=DIRECTION('ref_axis',(1.,0.,0.));
#5938=DIRECTION('center_axis',(0.,-1.,0.));
#5939=DIRECTION('ref_axis',(1.,0.,0.));
#5940=DIRECTION('',(0.,1.,0.));
#5941=DIRECTION('center_axis',(0.,1.,0.));
#5942=DIRECTION('ref_axis',(1.,0.,0.));
#5943=DIRECTION('center_axis',(0.,-1.,0.));
#5944=DIRECTION('ref_axis',(1.,0.,0.));
#5945=DIRECTION('center_axis',(0.,1.,0.));
#5946=DIRECTION('ref_axis',(1.,0.,0.));
#5947=DIRECTION('',(0.,-1.,0.));
#5948=DIRECTION('center_axis',(0.,-1.,0.));
#5949=DIRECTION('ref_axis',(1.,0.,0.));
#5950=DIRECTION('center_axis',(-0.4067366430758,0.,-0.913545457642601));
#5951=DIRECTION('ref_axis',(0.913545457642601,0.,-0.4067366430758));
#5952=DIRECTION('',(-0.913545457642601,0.,0.4067366430758));
#5953=DIRECTION('',(0.913545457642601,0.,-0.4067366430758));
#5954=DIRECTION('center_axis',(0.4067366430758,0.,0.913545457642601));
#5955=DIRECTION('ref_axis',(-0.913545457642601,0.,0.4067366430758));
#5956=DIRECTION('',(0.913545457642601,0.,-0.4067366430758));
#5957=DIRECTION('',(0.,1.,0.));
#5958=DIRECTION('',(-0.913545457642601,0.,0.4067366430758));
#5959=DIRECTION('',(0.,-1.,0.));
#5960=DIRECTION('center_axis',(0.,-1.,0.));
#5961=DIRECTION('ref_axis',(1.,0.,0.));
#5962=DIRECTION('center_axis',(0.,1.,0.));
#5963=DIRECTION('ref_axis',(1.,0.,0.));
#5964=DIRECTION('',(0.,1.,0.));
#5965=DIRECTION('center_axis',(0.,-1.,0.));
#5966=DIRECTION('ref_axis',(1.,0.,0.));
#5967=DIRECTION('center_axis',(0.,-1.,0.));
#5968=DIRECTION('ref_axis',(1.,0.,0.));
#5969=DIRECTION('center_axis',(0.,1.,0.));
#5970=DIRECTION('ref_axis',(1.,0.,0.));
#5971=DIRECTION('',(0.,-1.,0.));
#5972=DIRECTION('center_axis',(0.,-1.,0.));
#5973=DIRECTION('ref_axis',(1.,0.,0.));
#5974=DIRECTION('center_axis',(-0.951056516295154,0.,-0.309016994374948));
#5975=DIRECTION('ref_axis',(0.309016994374948,0.,-0.951056516295154));
#5976=DIRECTION('',(-0.309016994374948,0.,0.951056516295154));
#5977=DIRECTION('',(0.,1.,0.));
#5978=DIRECTION('',(0.309016994374948,0.,-0.951056516295154));
#5979=DIRECTION('',(0.,-1.,0.));
#5980=DIRECTION('center_axis',(0.951056516295154,0.,0.309016994374948));
#5981=DIRECTION('ref_axis',(-0.309016994374948,0.,0.951056516295154));
#5982=DIRECTION('',(0.309016994374948,0.,-0.951056516295154));
#5983=DIRECTION('',(-0.309016994374948,0.,0.951056516295154));
#5984=DIRECTION('center_axis',(0.,-1.,0.));
#5985=DIRECTION('ref_axis',(1.,0.,0.));
#5986=DIRECTION('center_axis',(0.,-1.,0.));
#5987=DIRECTION('ref_axis',(1.,0.,0.));
#5988=DIRECTION('',(0.,-1.,0.));
#5989=DIRECTION('center_axis',(0.,1.,0.));
#5990=DIRECTION('ref_axis',(1.,0.,0.));
#5991=DIRECTION('center_axis',(0.,-1.,0.));
#5992=DIRECTION('ref_axis',(1.,0.,0.));
#5993=DIRECTION('center_axis',(0.,-1.,0.));
#5994=DIRECTION('ref_axis',(1.,0.,0.));
#5995=DIRECTION('',(0.,1.,0.));
#5996=DIRECTION('center_axis',(0.,1.,0.));
#5997=DIRECTION('ref_axis',(1.,0.,0.));
#5998=DIRECTION('center_axis',(-0.846036043229222,0.,0.533125701459836));
#5999=DIRECTION('ref_axis',(-0.533125701459836,0.,-0.846036043229222));
#6000=DIRECTION('',(0.533125701459836,0.,0.846036043229222));
#6001=DIRECTION('',(0.,1.,0.));
#6002=DIRECTION('',(-0.533125701459836,0.,-0.846036043229222));
#6003=DIRECTION('',(0.,-1.,0.));
#6004=DIRECTION('center_axis',(0.395813852010064,0.,0.918330765332925));
#6005=DIRECTION('ref_axis',(-0.918330765332925,0.,0.395813852010064));
#6006=DIRECTION('',(0.918330765332925,0.,-0.395813852010064));
#6007=DIRECTION('',(-0.918330765332925,0.,0.395813852010064));
#6008=DIRECTION('',(0.,-1.,0.));
#6009=DIRECTION('center_axis',(0.971574977419217,0.,-0.236732049483902));
#6010=DIRECTION('ref_axis',(0.236732049483902,0.,0.971574977419217));
#6011=DIRECTION('',(-0.236732049483902,0.,-0.971574977419217));
#6012=DIRECTION('',(0.236732049483902,0.,0.971574977419217));
#6013=DIRECTION('',(0.,-1.,0.));
#6014=DIRECTION('center_axis',(0.,-1.,0.));
#6015=DIRECTION('ref_axis',(1.,0.,0.));
#6016=DIRECTION('center_axis',(0.,1.,0.));
#6017=DIRECTION('ref_axis',(1.,0.,0.));
#6018=DIRECTION('',(0.,-1.,0.));
#6019=DIRECTION('center_axis',(0.,-1.,0.));
#6020=DIRECTION('ref_axis',(1.,0.,0.));
#6021=DIRECTION('center_axis',(0.,-1.,0.));
#6022=DIRECTION('ref_axis',(1.,0.,0.));
#6023=DIRECTION('center_axis',(0.,-1.,0.));
#6024=DIRECTION('ref_axis',(1.,0.,0.));
#6025=DIRECTION('',(0.,1.,0.));
#6026=DIRECTION('center_axis',(0.,1.,0.));
#6027=DIRECTION('ref_axis',(1.,0.,0.));
#6028=DIRECTION('center_axis',(-0.99782096176235,0.,-0.0659797564989425));
#6029=DIRECTION('ref_axis',(0.0659797564989425,0.,-0.99782096176235));
#6030=DIRECTION('',(-0.0659797564989425,0.,0.997820961762349));
#6031=DIRECTION('',(0.,1.,0.));
#6032=DIRECTION('',(0.0659797564989425,0.,-0.997820961762349));
#6033=DIRECTION('',(0.,-1.,0.));
#6034=DIRECTION('center_axis',(-0.219561147704,0.,0.975598740476279));
#6035=DIRECTION('ref_axis',(-0.975598740476279,0.,-0.219561147704));
#6036=DIRECTION('',(0.975598740476279,0.,0.219561147704));
#6037=DIRECTION('',(-0.975598740476279,0.,-0.219561147704));
#6038=DIRECTION('',(0.,-1.,0.));
#6039=DIRECTION('center_axis',(0.925168275473212,0.,0.37955719207772));
#6040=DIRECTION('ref_axis',(-0.37955719207772,0.,0.925168275473212));
#6041=DIRECTION('',(0.37955719207772,0.,-0.925168275473212));
#6042=DIRECTION('',(-0.37955719207772,0.,0.925168275473212));
#6043=DIRECTION('',(0.,-1.,0.));
#6044=DIRECTION('center_axis',(0.,-1.,0.));
#6045=DIRECTION('ref_axis',(1.,0.,0.));
#6046=DIRECTION('center_axis',(0.,1.,0.));
#6047=DIRECTION('ref_axis',(1.,0.,0.));
#6048=DIRECTION('',(0.,-1.,0.));
#6049=DIRECTION('center_axis',(0.,-1.,0.));
#6050=DIRECTION('ref_axis',(1.,0.,0.));
#6051=DIRECTION('center_axis',(0.,-1.,0.));
#6052=DIRECTION('ref_axis',(1.,0.,0.));
#6053=DIRECTION('center_axis',(0.,-1.,0.));
#6054=DIRECTION('ref_axis',(1.,0.,0.));
#6055=DIRECTION('',(0.,1.,0.));
#6056=DIRECTION('center_axis',(0.,1.,0.));
#6057=DIRECTION('ref_axis',(1.,0.,0.));
#6058=DIRECTION('center_axis',(-0.98973414244318,0.,0.142920702776972));
#6059=DIRECTION('ref_axis',(-0.142920702776972,0.,-0.98973414244318));
#6060=DIRECTION('',(0.142920702776972,0.,0.98973414244318));
#6061=DIRECTION('',(-0.142920702776972,0.,-0.98973414244318));
#6062=DIRECTION('',(0.,-1.,0.));
#6063=DIRECTION('center_axis',(-0.0119248261489288,0.,0.999928896732822));
#6064=DIRECTION('ref_axis',(-0.999928896732822,0.,-0.0119248261489288));
#6065=DIRECTION('',(0.999928896732822,0.,0.0119248261489288));
#6066=DIRECTION('',(-0.999928896732822,0.,-0.0119248261489288));
#6067=DIRECTION('',(0.,-1.,0.));
#6068=DIRECTION('center_axis',(0.983865506496075,0.,0.178909656327496));
#6069=DIRECTION('ref_axis',(-0.178909656327496,0.,0.983865506496075));
#6070=DIRECTION('',(0.178909656327496,0.,-0.983865506496075));
#6071=DIRECTION('',(-0.178909656327496,0.,0.983865506496075));
#6072=DIRECTION('',(0.,-1.,0.));
#6073=DIRECTION('center_axis',(0.,-1.,0.));
#6074=DIRECTION('ref_axis',(1.,0.,0.));
#6075=DIRECTION('center_axis',(0.,-1.,0.));
#6076=DIRECTION('ref_axis',(1.,0.,0.));
#6077=DIRECTION('',(0.,1.,0.));
#6078=DIRECTION('center_axis',(0.,1.,0.));
#6079=DIRECTION('ref_axis',(1.,0.,0.));
#6080=DIRECTION('center_axis',(-0.938391191827905,0.,0.34557484153191));
#6081=DIRECTION('ref_axis',(-0.34557484153191,0.,-0.938391191827905));
#6082=DIRECTION('',(0.34557484153191,0.,0.938391191827905));
#6083=DIRECTION('',(-0.34557484153191,0.,-0.938391191827905));
#6084=DIRECTION('',(0.,-1.,0.));
#6085=DIRECTION('center_axis',(0.196232667530515,0.,0.980557362010943));
#6086=DIRECTION('ref_axis',(-0.980557362010943,0.,0.196232667530515));
#6087=DIRECTION('',(0.980557362010942,0.,-0.196232667530515));
#6088=DIRECTION('',(-0.980557362010942,0.,0.196232667530515));
#6089=DIRECTION('',(0.,-1.,0.));
#6090=DIRECTION('center_axis',(0.99956309377456,0.,-0.0295570899080193));
#6091=DIRECTION('ref_axis',(0.0295570899080193,0.,0.99956309377456));
#6092=DIRECTION('',(-0.0295570899080193,0.,-0.99956309377456));
#6093=DIRECTION('',(0.0295570899080193,0.,0.99956309377456));
#6094=DIRECTION('center_axis',(-0.716705059810067,0.,0.69737641001302));
#6095=DIRECTION('ref_axis',(-0.69737641001302,0.,-0.716705059810067));
#6096=DIRECTION('',(0.69737641001302,0.,0.716705059810067));
#6097=DIRECTION('',(-0.69737641001302,0.,-0.716705059810067));
#6098=DIRECTION('',(0.,-1.,0.));
#6099=DIRECTION('center_axis',(0.578096071831186,0.,0.815968707569937));
#6100=DIRECTION('ref_axis',(-0.815968707569937,0.,0.578096071831186));
#6101=DIRECTION('',(0.815968707569936,0.,-0.578096071831186));
#6102=DIRECTION('',(-0.815968707569936,0.,0.578096071831186));
#6103=DIRECTION('',(0.,-1.,0.));
#6104=DIRECTION('center_axis',(0.901124372416657,0.,-0.433560682530931));
#6105=DIRECTION('ref_axis',(0.433560682530931,0.,0.901124372416657));
#6106=DIRECTION('',(-0.433560682530931,0.,-0.901124372416657));
#6107=DIRECTION('',(0.433560682530931,0.,0.901124372416657));
#6108=DIRECTION('',(0.,-1.,0.));
#6109=DIRECTION('center_axis',(0.,-1.,0.));
#6110=DIRECTION('ref_axis',(1.,0.,0.));
#6111=DIRECTION('center_axis',(0.,-1.,0.));
#6112=DIRECTION('ref_axis',(1.,0.,0.));
#6113=DIRECTION('',(0.,1.,0.));
#6114=DIRECTION('center_axis',(0.,1.,0.));
#6115=DIRECTION('ref_axis',(1.,0.,0.));
#6116=DIRECTION('center_axis',(-0.556050626144771,0.,0.831148423065344));
#6117=DIRECTION('ref_axis',(-0.831148423065344,0.,-0.556050626144771));
#6118=DIRECTION('',(0.831148423065344,0.,0.556050626144771));
#6119=DIRECTION('',(-0.831148423065344,0.,-0.556050626144771));
#6120=DIRECTION('',(0.,-1.,0.));
#6121=DIRECTION('center_axis',(0.735112719300559,0.,0.677944901833871));
#6122=DIRECTION('ref_axis',(-0.677944901833871,0.,0.735112719300559));
#6123=DIRECTION('',(0.677944901833871,0.,-0.735112719300559));
#6124=DIRECTION('',(-0.677944901833871,0.,0.735112719300559));
#6125=DIRECTION('',(0.,-1.,0.));
#6126=DIRECTION('center_axis',(0.791290308265002,0.,-0.61144063329638));
#6127=DIRECTION('ref_axis',(0.61144063329638,0.,0.791290308265002));
#6128=DIRECTION('',(-0.61144063329638,0.,-0.791290308265002));
#6129=DIRECTION('',(0.61144063329638,0.,0.791290308265002));
#6130=DIRECTION('center_axis',(0.866025403784438,0.,0.5));
#6131=DIRECTION('ref_axis',(-0.5,0.,0.866025403784438));
#6132=DIRECTION('',(0.5,0.,-0.866025403784438));
#6133=DIRECTION('',(0.,1.,0.));
#6134=DIRECTION('',(-0.5,0.,0.866025403784438));
#6135=DIRECTION('',(0.,-1.,0.));
#6136=DIRECTION('center_axis',(-0.866025403784438,0.,-0.5));
#6137=DIRECTION('ref_axis',(0.5,0.,-0.866025403784438));
#6138=DIRECTION('',(-0.5,0.,0.866025403784438));
#6139=DIRECTION('',(0.,1.,0.));
#6140=DIRECTION('',(0.5,0.,-0.866025403784438));
#6141=DIRECTION('',(0.,-1.,0.));
#6142=DIRECTION('center_axis',(0.,-1.,0.));
#6143=DIRECTION('ref_axis',(1.,0.,0.));
#6144=DIRECTION('center_axis',(0.,-1.,0.));
#6145=DIRECTION('ref_axis',(1.,0.,0.));
#6146=DIRECTION('',(0.,-1.,0.));
#6147=DIRECTION('center_axis',(0.,1.,0.));
#6148=DIRECTION('ref_axis',(1.,0.,0.));
#6149=DIRECTION('center_axis',(0.,-1.,0.));
#6150=DIRECTION('ref_axis',(1.,0.,0.));
#6151=DIRECTION('center_axis',(0.,1.,0.));
#6152=DIRECTION('ref_axis',(1.,0.,0.));
#6153=DIRECTION('',(0.,1.,0.));
#6154=DIRECTION('center_axis',(0.,-1.,0.));
#6155=DIRECTION('ref_axis',(1.,0.,0.));
#6156=DIRECTION('center_axis',(0.,-1.,0.));
#6157=DIRECTION('ref_axis',(1.,0.,0.));
#6158=DIRECTION('center_axis',(0.,-1.,0.));
#6159=DIRECTION('ref_axis',(1.,0.,0.));
#6160=DIRECTION('',(0.,1.,0.));
#6161=DIRECTION('center_axis',(0.,1.,0.));
#6162=DIRECTION('ref_axis',(1.,0.,0.));
#6163=DIRECTION('center_axis',(0.,-1.,0.));
#6164=DIRECTION('ref_axis',(1.,0.,0.));
#6165=DIRECTION('center_axis',(0.,1.,0.));
#6166=DIRECTION('ref_axis',(1.,0.,0.));
#6167=DIRECTION('',(0.,-1.,0.));
#6168=DIRECTION('center_axis',(0.,-1.,0.));
#6169=DIRECTION('ref_axis',(1.,0.,0.));
#6170=DIRECTION('center_axis',(0.587785252292473,0.,0.809016994374948));
#6171=DIRECTION('ref_axis',(-0.809016994374948,0.,0.587785252292473));
#6172=DIRECTION('',(0.809016994374947,0.,-0.587785252292473));
#6173=DIRECTION('',(-0.809016994374947,0.,0.587785252292473));
#6174=DIRECTION('center_axis',(-0.587785252292473,0.,-0.809016994374948));
#6175=DIRECTION('ref_axis',(0.809016994374948,0.,-0.587785252292473));
#6176=DIRECTION('',(-0.809016994374947,0.,0.587785252292473));
#6177=DIRECTION('',(0.,1.,0.));
#6178=DIRECTION('',(0.809016994374947,0.,-0.587785252292473));
#6179=DIRECTION('',(0.,-1.,0.));
#6180=DIRECTION('center_axis',(0.,-1.,0.));
#6181=DIRECTION('ref_axis',(1.,0.,0.));
#6182=DIRECTION('center_axis',(0.,1.,0.));
#6183=DIRECTION('ref_axis',(1.,0.,0.));
#6184=DIRECTION('',(0.,1.,0.));
#6185=DIRECTION('center_axis',(0.,-1.,0.));
#6186=DIRECTION('ref_axis',(1.,0.,0.));
#6187=DIRECTION('center_axis',(0.,-1.,0.));
#6188=DIRECTION('ref_axis',(1.,0.,0.));
#6189=DIRECTION('center_axis',(0.,1.,0.));
#6190=DIRECTION('ref_axis',(1.,0.,0.));
#6191=DIRECTION('',(0.,-1.,0.));
#6192=DIRECTION('center_axis',(0.,-1.,0.));
#6193=DIRECTION('ref_axis',(1.,0.,0.));
#6194=DIRECTION('center_axis',(0.951056516295154,0.,-0.309016994374947));
#6195=DIRECTION('ref_axis',(0.309016994374947,0.,0.951056516295154));
#6196=DIRECTION('',(-0.309016994374947,0.,-0.951056516295154));
#6197=DIRECTION('',(0.,1.,0.));
#6198=DIRECTION('',(0.309016994374947,0.,0.951056516295154));
#6199=DIRECTION('',(0.,-1.,0.));
#6200=DIRECTION('center_axis',(-0.951056516295154,0.,0.309016994374947));
#6201=DIRECTION('ref_axis',(-0.309016994374947,0.,-0.951056516295154));
#6202=DIRECTION('',(0.309016994374947,0.,0.951056516295154));
#6203=DIRECTION('',(0.,1.,0.));
#6204=DIRECTION('',(-0.309016994374947,0.,-0.951056516295154));
#6205=DIRECTION('',(0.,-1.,0.));
#6206=DIRECTION('center_axis',(0.,-1.,0.));
#6207=DIRECTION('ref_axis',(1.,0.,0.));
#6208=DIRECTION('center_axis',(0.,-1.,0.));
#6209=DIRECTION('ref_axis',(1.,0.,0.));
#6210=DIRECTION('',(0.,-1.,0.));
#6211=DIRECTION('center_axis',(0.,1.,0.));
#6212=DIRECTION('ref_axis',(1.,0.,0.));
#6213=DIRECTION('center_axis',(0.,-1.,0.));
#6214=DIRECTION('ref_axis',(1.,0.,0.));
#6215=DIRECTION('center_axis',(0.,1.,0.));
#6216=DIRECTION('ref_axis',(1.,0.,0.));
#6217=DIRECTION('',(0.,1.,0.));
#6218=DIRECTION('center_axis',(0.,-1.,0.));
#6219=DIRECTION('ref_axis',(1.,0.,0.));
#6220=DIRECTION('center_axis',(0.,-1.,0.));
#6221=DIRECTION('ref_axis',(1.,0.,0.));
#6222=DIRECTION('center_axis',(0.,-1.,0.));
#6223=DIRECTION('ref_axis',(1.,0.,0.));
#6224=DIRECTION('',(0.,1.,0.));
#6225=DIRECTION('center_axis',(0.,1.,0.));
#6226=DIRECTION('ref_axis',(1.,0.,0.));
#6227=DIRECTION('center_axis',(0.,-1.,0.));
#6228=DIRECTION('ref_axis',(1.,0.,0.));
#6229=DIRECTION('center_axis',(0.,1.,0.));
#6230=DIRECTION('ref_axis',(1.,0.,0.));
#6231=DIRECTION('',(0.,-1.,0.));
#6232=DIRECTION('center_axis',(0.,-1.,0.));
#6233=DIRECTION('ref_axis',(1.,0.,0.));
#6234=DIRECTION('center_axis',(0.406736643075801,0.,-0.913545457642601));
#6235=DIRECTION('ref_axis',(0.913545457642601,0.,0.406736643075801));
#6236=DIRECTION('',(-0.913545457642601,0.,-0.406736643075801));
#6237=DIRECTION('',(0.,1.,0.));
#6238=DIRECTION('',(0.913545457642601,0.,0.406736643075801));
#6239=DIRECTION('',(0.,-1.,0.));
#6240=DIRECTION('center_axis',(-0.406736643075801,0.,0.913545457642601));
#6241=DIRECTION('ref_axis',(-0.913545457642601,0.,-0.406736643075801));
#6242=DIRECTION('',(0.913545457642601,0.,0.406736643075801));
#6243=DIRECTION('',(0.,1.,0.));
#6244=DIRECTION('',(-0.913545457642601,0.,-0.406736643075801));
#6245=DIRECTION('',(0.,-1.,0.));
#6246=DIRECTION('center_axis',(0.,-1.,0.));
#6247=DIRECTION('ref_axis',(1.,0.,0.));
#6248=DIRECTION('center_axis',(0.,-1.,0.));
#6249=DIRECTION('ref_axis',(1.,0.,0.));
#6250=DIRECTION('',(0.,-1.,0.));
#6251=DIRECTION('center_axis',(0.,1.,0.));
#6252=DIRECTION('ref_axis',(1.,0.,0.));
#6253=DIRECTION('center_axis',(0.,-1.,0.));
#6254=DIRECTION('ref_axis',(1.,0.,0.));
#6255=DIRECTION('center_axis',(0.,1.,0.));
#6256=DIRECTION('ref_axis',(1.,0.,0.));
#6257=DIRECTION('',(0.,1.,0.));
#6258=DIRECTION('center_axis',(0.,-1.,0.));
#6259=DIRECTION('ref_axis',(1.,0.,0.));
#6260=DIRECTION('center_axis',(0.,-1.,0.));
#6261=DIRECTION('ref_axis',(1.,0.,0.));
#6262=DIRECTION('center_axis',(0.,-1.,0.));
#6263=DIRECTION('ref_axis',(1.,0.,0.));
#6264=DIRECTION('',(0.,1.,0.));
#6265=DIRECTION('center_axis',(0.,1.,0.));
#6266=DIRECTION('ref_axis',(1.,0.,0.));
#6267=DIRECTION('center_axis',(0.,-1.,0.));
#6268=DIRECTION('ref_axis',(1.,0.,0.));
#6269=DIRECTION('center_axis',(0.,1.,0.));
#6270=DIRECTION('ref_axis',(1.,0.,0.));
#6271=DIRECTION('',(0.,-1.,0.));
#6272=DIRECTION('center_axis',(0.,-1.,0.));
#6273=DIRECTION('ref_axis',(1.,0.,0.));
#6274=DIRECTION('center_axis',(0.207911690817759,0.,0.978147600733806));
#6275=DIRECTION('ref_axis',(-0.978147600733806,0.,0.207911690817759));
#6276=DIRECTION('',(0.978147600733806,0.,-0.207911690817759));
#6277=DIRECTION('',(-0.978147600733806,0.,0.207911690817759));
#6278=DIRECTION('center_axis',(-0.207911690817759,0.,-0.978147600733806));
#6279=DIRECTION('ref_axis',(0.978147600733806,0.,-0.207911690817759));
#6280=DIRECTION('',(-0.978147600733806,0.,0.207911690817759));
#6281=DIRECTION('',(0.,1.,0.));
#6282=DIRECTION('',(0.978147600733806,0.,-0.207911690817759));
#6283=DIRECTION('',(0.,-1.,0.));
#6284=DIRECTION('center_axis',(0.,-1.,0.));
#6285=DIRECTION('ref_axis',(-1.,0.,1.22464679914735E-16));
#6286=DIRECTION('center_axis',(0.,1.,0.));
#6287=DIRECTION('ref_axis',(1.,0.,0.));
#6288=DIRECTION('',(0.,1.,0.));
#6289=DIRECTION('center_axis',(0.,-1.,0.));
#6290=DIRECTION('ref_axis',(1.,0.,0.));
#6291=DIRECTION('center_axis',(0.,-1.,0.));
#6292=DIRECTION('ref_axis',(-1.,0.,5.66553889764798E-16));
#6293=DIRECTION('center_axis',(0.,1.,0.));
#6294=DIRECTION('ref_axis',(1.,0.,0.));
#6295=DIRECTION('',(0.,-1.,0.));
#6296=DIRECTION('center_axis',(0.,-1.,0.));
#6297=DIRECTION('ref_axis',(1.,0.,0.));
#6298=DIRECTION('center_axis',(0.743144825477395,0.,-0.669130606358858));
#6299=DIRECTION('ref_axis',(0.669130606358858,0.,0.743144825477395));
#6300=DIRECTION('',(-0.669130606358858,0.,-0.743144825477395));
#6301=DIRECTION('',(0.669130606358858,0.,0.743144825477395));
#6302=DIRECTION('center_axis',(-0.743144825477395,0.,0.669130606358858));
#6303=DIRECTION('ref_axis',(-0.669130606358858,0.,-0.743144825477395));
#6304=DIRECTION('',(0.669130606358858,0.,0.743144825477395));
#6305=DIRECTION('',(-0.669130606358858,0.,-0.743144825477395));
#6306=DIRECTION('center_axis',(-0.20791169081776,0.,0.978147600733806));
#6307=DIRECTION('ref_axis',(-0.978147600733805,0.,-0.20791169081776));
#6308=DIRECTION('',(0.978147600733805,0.,0.20791169081776));
#6309=DIRECTION('',(-0.978147600733805,0.,-0.20791169081776));
#6310=DIRECTION('center_axis',(0.20791169081776,0.,-0.978147600733806));
#6311=DIRECTION('ref_axis',(0.978147600733805,0.,0.20791169081776));
#6312=DIRECTION('',(-0.978147600733805,0.,-0.20791169081776));
#6313=DIRECTION('',(0.,1.,0.));
#6314=DIRECTION('',(0.978147600733805,0.,0.20791169081776));
#6315=DIRECTION('',(0.,-1.,0.));
#6316=DIRECTION('center_axis',(0.,-1.,0.));
#6317=DIRECTION('ref_axis',(1.,0.,0.));
#6318=DIRECTION('center_axis',(0.,1.,0.));
#6319=DIRECTION('ref_axis',(1.,0.,0.));
#6320=DIRECTION('',(0.,1.,0.));
#6321=DIRECTION('center_axis',(0.,-1.,0.));
#6322=DIRECTION('ref_axis',(1.,0.,0.));
#6323=DIRECTION('center_axis',(0.,-1.,0.));
#6324=DIRECTION('ref_axis',(1.,0.,0.));
#6325=DIRECTION('center_axis',(0.,1.,0.));
#6326=DIRECTION('ref_axis',(1.,0.,0.));
#6327=DIRECTION('',(0.,-1.,0.));
#6328=DIRECTION('center_axis',(0.,-1.,0.));
#6329=DIRECTION('ref_axis',(1.,0.,0.));
#6330=DIRECTION('center_axis',(0.994521895368273,0.,0.104528463267654));
#6331=DIRECTION('ref_axis',(-0.104528463267654,0.,0.994521895368273));
#6332=DIRECTION('',(0.104528463267654,0.,-0.994521895368273));
#6333=DIRECTION('',(-0.104528463267654,0.,0.994521895368273));
#6334=DIRECTION('center_axis',(-0.994521895368273,0.,-0.104528463267654));
#6335=DIRECTION('ref_axis',(0.104528463267654,0.,-0.994521895368273));
#6336=DIRECTION('',(-0.104528463267654,0.,0.994521895368273));
#6337=DIRECTION('',(0.104528463267654,0.,-0.994521895368273));
#6338=DIRECTION('center_axis',(0.99782096176235,0.,0.0659797564989427));
#6339=DIRECTION('ref_axis',(-0.0659797564989427,0.,0.99782096176235));
#6340=DIRECTION('',(0.0659797564989427,0.,-0.997820961762349));
#6341=DIRECTION('',(0.,1.,0.));
#6342=DIRECTION('',(-0.0659797564989426,0.,0.997820961762349));
#6343=DIRECTION('',(0.,-1.,0.));
#6344=DIRECTION('center_axis',(0.219561147704001,0.,-0.975598740476279));
#6345=DIRECTION('ref_axis',(0.975598740476279,0.,0.219561147704001));
#6346=DIRECTION('',(-0.975598740476279,0.,-0.219561147704001));
#6347=DIRECTION('',(0.975598740476279,0.,0.219561147704001));
#6348=DIRECTION('',(0.,-1.,0.));
#6349=DIRECTION('center_axis',(-0.925168275473212,0.,-0.379557192077721));
#6350=DIRECTION('ref_axis',(0.379557192077721,0.,-0.925168275473212));
#6351=DIRECTION('',(-0.379557192077721,0.,0.925168275473211));
#6352=DIRECTION('',(0.379557192077721,0.,-0.925168275473211));
#6353=DIRECTION('',(0.,-1.,0.));
#6354=DIRECTION('center_axis',(0.,-1.,0.));
#6355=DIRECTION('ref_axis',(1.,0.,0.));
#6356=DIRECTION('center_axis',(0.,1.,0.));
#6357=DIRECTION('ref_axis',(1.,0.,0.));
#6358=DIRECTION('',(0.,-1.,0.));
#6359=DIRECTION('center_axis',(0.,-1.,0.));
#6360=DIRECTION('ref_axis',(1.,0.,0.));
#6361=DIRECTION('center_axis',(0.,-1.,0.));
#6362=DIRECTION('ref_axis',(1.,0.,0.));
#6363=DIRECTION('center_axis',(0.,-1.,0.));
#6364=DIRECTION('ref_axis',(1.,0.,0.));
#6365=DIRECTION('',(0.,1.,0.));
#6366=DIRECTION('center_axis',(0.,1.,0.));
#6367=DIRECTION('ref_axis',(1.,0.,0.));
#6368=DIRECTION('center_axis',(0.98973414244318,0.,-0.142920702776971));
#6369=DIRECTION('ref_axis',(0.142920702776971,0.,0.98973414244318));
#6370=DIRECTION('',(-0.142920702776971,0.,-0.98973414244318));
#6371=DIRECTION('',(0.142920702776971,0.,0.98973414244318));
#6372=DIRECTION('',(0.,-1.,0.));
#6373=DIRECTION('center_axis',(0.0119248261489294,0.,-0.999928896732822));
#6374=DIRECTION('ref_axis',(0.999928896732822,0.,0.0119248261489294));
#6375=DIRECTION('',(-0.999928896732822,0.,-0.0119248261489294));
#6376=DIRECTION('',(0.999928896732822,0.,0.0119248261489294));
#6377=DIRECTION('',(0.,-1.,0.));
#6378=DIRECTION('center_axis',(-0.983865506496074,0.,-0.178909656327497));
#6379=DIRECTION('ref_axis',(0.178909656327497,0.,-0.983865506496074));
#6380=DIRECTION('',(-0.178909656327497,0.,0.983865506496074));
#6381=DIRECTION('',(0.178909656327497,0.,-0.983865506496074));
#6382=DIRECTION('',(0.,-1.,0.));
#6383=DIRECTION('center_axis',(0.,-1.,0.));
#6384=DIRECTION('ref_axis',(1.,0.,0.));
#6385=DIRECTION('center_axis',(0.,-1.,0.));
#6386=DIRECTION('ref_axis',(1.,0.,0.));
#6387=DIRECTION('',(0.,1.,0.));
#6388=DIRECTION('center_axis',(0.,1.,0.));
#6389=DIRECTION('ref_axis',(1.,0.,0.));
#6390=DIRECTION('center_axis',(0.846036043229222,0.,-0.533125701459835));
#6391=DIRECTION('ref_axis',(0.533125701459835,0.,0.846036043229222));
#6392=DIRECTION('',(-0.533125701459835,0.,-0.846036043229222));
#6393=DIRECTION('',(0.,1.,0.));
#6394=DIRECTION('',(0.533125701459835,0.,0.846036043229222));
#6395=DIRECTION('',(0.,-1.,0.));
#6396=DIRECTION('center_axis',(-0.395813852010064,0.,-0.918330765332925));
#6397=DIRECTION('ref_axis',(0.918330765332925,0.,-0.395813852010064));
#6398=DIRECTION('',(-0.918330765332925,0.,0.395813852010064));
#6399=DIRECTION('',(0.918330765332925,0.,-0.395813852010064));
#6400=DIRECTION('',(0.,-1.,0.));
#6401=DIRECTION('center_axis',(-0.971574977419217,0.,0.236732049483902));
#6402=DIRECTION('ref_axis',(-0.236732049483902,0.,-0.971574977419217));
#6403=DIRECTION('',(0.236732049483902,0.,0.971574977419217));
#6404=DIRECTION('',(-0.236732049483902,0.,-0.971574977419217));
#6405=DIRECTION('',(0.,-1.,0.));
#6406=DIRECTION('center_axis',(0.,-1.,0.));
#6407=DIRECTION('ref_axis',(1.,0.,0.));
#6408=DIRECTION('center_axis',(0.,1.,0.));
#6409=DIRECTION('ref_axis',(1.,0.,0.));
#6410=DIRECTION('',(0.,-1.,0.));
#6411=DIRECTION('center_axis',(0.,-1.,0.));
#6412=DIRECTION('ref_axis',(1.,0.,0.));
#6413=DIRECTION('center_axis',(0.,-1.,0.));
#6414=DIRECTION('ref_axis',(1.,0.,0.));
#6415=DIRECTION('center_axis',(0.,-1.,0.));
#6416=DIRECTION('ref_axis',(1.,0.,0.));
#6417=DIRECTION('',(0.,1.,0.));
#6418=DIRECTION('center_axis',(0.,1.,0.));
#6419=DIRECTION('ref_axis',(1.,0.,0.));
#6420=DIRECTION('center_axis',(0.556050626144771,0.,-0.831148423065344));
#6421=DIRECTION('ref_axis',(0.831148423065344,0.,0.556050626144771));
#6422=DIRECTION('',(-0.831148423065344,0.,-0.556050626144771));
#6423=DIRECTION('',(0.,1.,0.));
#6424=DIRECTION('',(0.831148423065344,0.,0.556050626144771));
#6425=DIRECTION('',(0.,-1.,0.));
#6426=DIRECTION('center_axis',(-0.735112719300559,0.,-0.677944901833872));
#6427=DIRECTION('ref_axis',(0.677944901833872,0.,-0.735112719300559));
#6428=DIRECTION('',(-0.677944901833872,0.,0.735112719300559));
#6429=DIRECTION('',(0.677944901833871,0.,-0.735112719300559));
#6430=DIRECTION('',(0.,-1.,0.));
#6431=DIRECTION('center_axis',(-0.791290308265002,0.,0.61144063329638));
#6432=DIRECTION('ref_axis',(-0.61144063329638,0.,-0.791290308265002));
#6433=DIRECTION('',(0.61144063329638,0.,0.791290308265002));
#6434=DIRECTION('',(-0.61144063329638,0.,-0.791290308265002));
#6435=DIRECTION('',(0.,-1.,0.));
#6436=DIRECTION('center_axis',(0.,-1.,0.));
#6437=DIRECTION('ref_axis',(1.,0.,0.));
#6438=DIRECTION('center_axis',(0.,1.,0.));
#6439=DIRECTION('ref_axis',(1.,0.,0.));
#6440=DIRECTION('',(0.,-1.,0.));
#6441=DIRECTION('center_axis',(0.,-1.,0.));
#6442=DIRECTION('ref_axis',(1.,0.,0.));
#6443=DIRECTION('center_axis',(0.,-1.,0.));
#6444=DIRECTION('ref_axis',(1.,0.,0.));
#6445=DIRECTION('center_axis',(0.,-1.,0.));
#6446=DIRECTION('ref_axis',(1.,0.,0.));
#6447=DIRECTION('',(0.,1.,0.));
#6448=DIRECTION('center_axis',(0.,1.,0.));
#6449=DIRECTION('ref_axis',(1.,0.,0.));
#6450=DIRECTION('center_axis',(0.716705059810068,0.,-0.69737641001302));
#6451=DIRECTION('ref_axis',(0.69737641001302,0.,0.716705059810068));
#6452=DIRECTION('',(-0.69737641001302,0.,-0.716705059810068));
#6453=DIRECTION('',(0.69737641001302,0.,0.716705059810068));
#6454=DIRECTION('',(0.,-1.,0.));
#6455=DIRECTION('center_axis',(-0.578096071831185,0.,-0.815968707569937));
#6456=DIRECTION('ref_axis',(0.815968707569937,0.,-0.578096071831185));
#6457=DIRECTION('',(-0.815968707569937,0.,0.578096071831185));
#6458=DIRECTION('',(0.815968707569937,0.,-0.578096071831185));
#6459=DIRECTION('',(0.,-1.,0.));
#6460=DIRECTION('center_axis',(-0.901124372416657,0.,0.433560682530931));
#6461=DIRECTION('ref_axis',(-0.433560682530931,0.,-0.901124372416657));
#6462=DIRECTION('',(0.433560682530931,0.,0.901124372416657));
#6463=DIRECTION('',(-0.433560682530931,0.,-0.901124372416657));
#6464=DIRECTION('center_axis',(0.962298216976301,0.,0.271996583809855));
#6465=DIRECTION('ref_axis',(-0.271996583809855,0.,0.962298216976301));
#6466=DIRECTION('',(0.271996583809855,0.,-0.962298216976301));
#6467=DIRECTION('',(-0.271996583809855,0.,0.962298216976301));
#6468=DIRECTION('',(0.,-1.,0.));
#6469=DIRECTION('center_axis',(0.417601593533129,0.,-0.908630237818768));
#6470=DIRECTION('ref_axis',(0.908630237818768,0.,0.417601593533129));
#6471=DIRECTION('',(-0.908630237818768,0.,-0.417601593533129));
#6472=DIRECTION('',(0.908630237818768,0.,0.417601593533129));
#6473=DIRECTION('',(0.,-1.,0.));
#6474=DIRECTION('center_axis',(-0.826036751362234,0.,-0.563616257216669));
#6475=DIRECTION('ref_axis',(0.563616257216669,0.,-0.826036751362234));
#6476=DIRECTION('',(-0.563616257216669,0.,0.826036751362234));
#6477=DIRECTION('',(0.563616257216669,0.,-0.826036751362234));
#6478=DIRECTION('center_axis',(0.938391191827905,0.,-0.34557484153191));
#6479=DIRECTION('ref_axis',(0.34557484153191,0.,0.938391191827905));
#6480=DIRECTION('',(-0.34557484153191,0.,-0.938391191827905));
#6481=DIRECTION('',(0.34557484153191,0.,0.938391191827905));
#6482=DIRECTION('',(0.,-1.,0.));
#6483=DIRECTION('center_axis',(-0.196232667530514,0.,-0.980557362010943));
#6484=DIRECTION('ref_axis',(0.980557362010943,0.,-0.196232667530514));
#6485=DIRECTION('',(-0.980557362010943,0.,0.196232667530514));
#6486=DIRECTION('',(0.980557362010943,0.,-0.196232667530514));
#6487=DIRECTION('',(0.,-1.,0.));
#6488=DIRECTION('center_axis',(-0.99956309377456,0.,0.0295570899080193));
#6489=DIRECTION('ref_axis',(-0.0295570899080193,0.,-0.99956309377456));
#6490=DIRECTION('',(0.0295570899080193,0.,0.99956309377456));
#6491=DIRECTION('',(-0.0295570899080193,0.,-0.99956309377456));
#6492=DIRECTION('center_axis',(0.371094111890008,0.,-0.928595261737086));
#6493=DIRECTION('ref_axis',(0.928595261737086,0.,0.371094111890008));
#6494=DIRECTION('',(-0.928595261737086,0.,-0.371094111890008));
#6495=DIRECTION('',(0.928595261737086,0.,0.371094111890008));
#6496=DIRECTION('',(0.,-1.,0.));
#6497=DIRECTION('center_axis',(-0.860001413474305,0.,-0.510291650747097));
#6498=DIRECTION('ref_axis',(0.510291650747097,0.,-0.860001413474305));
#6499=DIRECTION('',(-0.510291650747097,0.,0.860001413474305));
#6500=DIRECTION('',(0.510291650747097,0.,-0.860001413474305));
#6501=DIRECTION('',(0.,-1.,0.));
#6502=DIRECTION('center_axis',(-0.646873060609993,0.,0.762597694369096));
#6503=DIRECTION('ref_axis',(-0.762597694369096,0.,-0.646873060609993));
#6504=DIRECTION('',(0.762597694369096,0.,0.646873060609993));
#6505=DIRECTION('',(-0.762597694369096,0.,-0.646873060609993));
#6506=DIRECTION('',(0.,-1.,0.));
#6507=DIRECTION('center_axis',(0.,-1.,0.));
#6508=DIRECTION('ref_axis',(1.,0.,0.));
#6509=DIRECTION('center_axis',(0.,-1.,0.));
#6510=DIRECTION('ref_axis',(1.,0.,0.));
#6511=DIRECTION('',(0.,1.,0.));
#6512=DIRECTION('center_axis',(0.,1.,0.));
#6513=DIRECTION('ref_axis',(1.,0.,0.));
#6514=DIRECTION('center_axis',(-0.587785252292473,0.,0.809016994374947));
#6515=DIRECTION('ref_axis',(-0.809016994374947,0.,-0.587785252292473));
#6516=DIRECTION('',(0.809016994374947,0.,0.587785252292473));
#6517=DIRECTION('',(-0.809016994374947,0.,-0.587785252292473));
#6518=DIRECTION('center_axis',(0.587785252292473,0.,-0.809016994374947));
#6519=DIRECTION('ref_axis',(0.809016994374947,0.,0.587785252292473));
#6520=DIRECTION('',(-0.809016994374947,0.,-0.587785252292473));
#6521=DIRECTION('',(0.,1.,0.));
#6522=DIRECTION('',(0.809016994374947,0.,0.587785252292473));
#6523=DIRECTION('',(0.,-1.,0.));
#6524=DIRECTION('center_axis',(0.,-1.,0.));
#6525=DIRECTION('ref_axis',(1.,0.,0.));
#6526=DIRECTION('center_axis',(0.,1.,0.));
#6527=DIRECTION('ref_axis',(1.,0.,0.));
#6528=DIRECTION('',(0.,1.,0.));
#6529=DIRECTION('center_axis',(0.,-1.,0.));
#6530=DIRECTION('ref_axis',(1.,0.,0.));
#6531=DIRECTION('center_axis',(0.,-1.,0.));
#6532=DIRECTION('ref_axis',(1.,0.,0.));
#6533=DIRECTION('center_axis',(0.,1.,0.));
#6534=DIRECTION('ref_axis',(1.,0.,0.));
#6535=DIRECTION('',(0.,-1.,0.));
#6536=DIRECTION('center_axis',(0.,-1.,0.));
#6537=DIRECTION('ref_axis',(1.,0.,0.));
#6538=DIRECTION('center_axis',(-0.994521895368273,0.,0.104528463267653));
#6539=DIRECTION('ref_axis',(-0.104528463267653,0.,-0.994521895368273));
#6540=DIRECTION('',(0.104528463267653,0.,0.994521895368273));
#6541=DIRECTION('',(0.,1.,0.));
#6542=DIRECTION('',(-0.104528463267653,0.,-0.994521895368273));
#6543=DIRECTION('',(0.,-1.,0.));
#6544=DIRECTION('center_axis',(0.994521895368273,0.,-0.104528463267653));
#6545=DIRECTION('ref_axis',(0.104528463267653,0.,0.994521895368273));
#6546=DIRECTION('',(-0.104528463267653,0.,-0.994521895368273));
#6547=DIRECTION('',(0.104528463267653,0.,0.994521895368273));
#6548=DIRECTION('center_axis',(0.,-1.,0.));
#6549=DIRECTION('ref_axis',(1.,0.,0.));
#6550=DIRECTION('center_axis',(0.,-1.,0.));
#6551=DIRECTION('ref_axis',(1.,0.,0.));
#6552=DIRECTION('',(0.,-1.,0.));
#6553=DIRECTION('center_axis',(0.,1.,0.));
#6554=DIRECTION('ref_axis',(1.,0.,0.));
#6555=DIRECTION('center_axis',(0.,-1.,0.));
#6556=DIRECTION('ref_axis',(1.,0.,0.));
#6557=DIRECTION('center_axis',(0.,-1.,0.));
#6558=DIRECTION('ref_axis',(1.,0.,0.));
#6559=DIRECTION('',(0.,1.,0.));
#6560=DIRECTION('center_axis',(0.,1.,0.));
#6561=DIRECTION('ref_axis',(1.,0.,0.));
#6562=DIRECTION('center_axis',(-0.866025403784439,0.,0.5));
#6563=DIRECTION('ref_axis',(-0.5,0.,-0.866025403784439));
#6564=DIRECTION('',(0.5,0.,0.866025403784439));
#6565=DIRECTION('',(-0.5,0.,-0.866025403784439));
#6566=DIRECTION('center_axis',(0.866025403784439,0.,-0.5));
#6567=DIRECTION('ref_axis',(0.5,0.,0.866025403784439));
#6568=DIRECTION('',(-0.5,0.,-0.866025403784439));
#6569=DIRECTION('',(0.5,0.,0.866025403784439));
#6570=DIRECTION('center_axis',(-0.245593157166233,0.,-0.969372993822874));
#6571=DIRECTION('ref_axis',(0.969372993822874,0.,-0.245593157166233));
#6572=DIRECTION('',(-0.969372993822874,0.,0.245593157166233));
#6573=DIRECTION('',(0.,1.,0.));
#6574=DIRECTION('',(0.969372993822874,0.,-0.245593157166233));
#6575=DIRECTION('',(0.,-1.,0.));
#6576=DIRECTION('center_axis',(-0.995697665364314,0.,0.0926615302488315));
#6577=DIRECTION('ref_axis',(-0.0926615302488315,0.,-0.995697665364314));
#6578=DIRECTION('',(0.0926615302488314,0.,0.995697665364314));
#6579=DIRECTION('',(-0.0926615302488314,0.,-0.995697665364314));
#6580=DIRECTION('',(0.,-1.,0.));
#6581=DIRECTION('center_axis',(-0.0750876210544224,0.,0.997176939747599));
#6582=DIRECTION('ref_axis',(-0.997176939747599,0.,-0.0750876210544224));
#6583=DIRECTION('',(0.997176939747599,0.,0.0750876210544224));
#6584=DIRECTION('',(-0.997176939747599,0.,-0.0750876210544224));
#6585=DIRECTION('',(0.,-1.,0.));
#6586=DIRECTION('center_axis',(0.,-1.,0.));
#6587=DIRECTION('ref_axis',(1.,0.,0.));
#6588=DIRECTION('center_axis',(0.,1.,0.));
#6589=DIRECTION('ref_axis',(1.,0.,0.));
#6590=DIRECTION('',(0.,-1.,0.));
#6591=DIRECTION('center_axis',(0.,-1.,0.));
#6592=DIRECTION('ref_axis',(1.,0.,0.));
#6593=DIRECTION('center_axis',(0.,-1.,0.));
#6594=DIRECTION('ref_axis',(1.,0.,0.));
#6595=DIRECTION('center_axis',(0.,-1.,0.));
#6596=DIRECTION('ref_axis',(1.,0.,0.));
#6597=DIRECTION('',(0.,1.,0.));
#6598=DIRECTION('center_axis',(0.,1.,0.));
#6599=DIRECTION('ref_axis',(1.,0.,0.));
#6600=DIRECTION('center_axis',(-0.441770335617579,0.,-0.897128179564287));
#6601=DIRECTION('ref_axis',(0.897128179564287,0.,-0.441770335617579));
#6602=DIRECTION('',(-0.897128179564287,0.,0.441770335617579));
#6603=DIRECTION('',(0.897128179564287,0.,-0.441770335617579));
#6604=DIRECTION('',(0.,-1.,0.));
#6605=DIRECTION('center_axis',(-0.95467386700456,0.,0.297653838642407));
#6606=DIRECTION('ref_axis',(-0.297653838642407,0.,-0.95467386700456));
#6607=DIRECTION('',(0.297653838642407,0.,0.95467386700456));
#6608=DIRECTION('',(-0.297653838642407,0.,-0.95467386700456));
#6609=DIRECTION('',(0.,-1.,0.));
#6610=DIRECTION('center_axis',(0.13387796720821,0.,0.990997825374101));
#6611=DIRECTION('ref_axis',(-0.990997825374101,0.,0.13387796720821));
#6612=DIRECTION('',(0.990997825374101,0.,-0.13387796720821));
#6613=DIRECTION('',(-0.990997825374101,0.,0.13387796720821));
#6614=DIRECTION('',(0.,-1.,0.));
#6615=DIRECTION('center_axis',(0.,-1.,0.));
#6616=DIRECTION('ref_axis',(1.,0.,0.));
#6617=DIRECTION('center_axis',(0.,-1.,0.));
#6618=DIRECTION('ref_axis',(1.,0.,0.));
#6619=DIRECTION('',(0.,1.,0.));
#6620=DIRECTION('center_axis',(0.,1.,0.));
#6621=DIRECTION('ref_axis',(1.,0.,0.));
#6622=DIRECTION('center_axis',(-0.884718422489227,0.,-0.466125855223859));
#6623=DIRECTION('ref_axis',(0.466125855223859,0.,-0.884718422489227));
#6624=DIRECTION('',(-0.466125855223859,0.,0.884718422489227));
#6625=DIRECTION('',(0.,1.,0.));
#6626=DIRECTION('',(0.466125855223859,0.,-0.884718422489227));
#6627=DIRECTION('',(0.,-1.,0.));
#6628=DIRECTION('center_axis',(-0.597390845850087,0.,0.801950233676952));
#6629=DIRECTION('ref_axis',(-0.801950233676952,0.,-0.597390845850087));
#6630=DIRECTION('',(0.801950233676952,0.,0.597390845850087));
#6631=DIRECTION('',(-0.801950233676952,0.,-0.597390845850087));
#6632=DIRECTION('',(0.,-1.,0.));
#6633=DIRECTION('center_axis',(0.690803457452622,0.,0.723042587384383));
#6634=DIRECTION('ref_axis',(-0.723042587384383,0.,0.690803457452622));
#6635=DIRECTION('',(0.723042587384383,0.,-0.690803457452622));
#6636=DIRECTION('',(-0.723042587384383,0.,0.690803457452622));
#6637=DIRECTION('',(0.,-1.,0.));
#6638=DIRECTION('center_axis',(0.,-1.,0.));
#6639=DIRECTION('ref_axis',(1.,0.,0.));
#6640=DIRECTION('center_axis',(0.,1.,0.));
#6641=DIRECTION('ref_axis',(1.,0.,0.));
#6642=DIRECTION('',(0.,-1.,0.));
#6643=DIRECTION('center_axis',(0.,-1.,0.));
#6644=DIRECTION('ref_axis',(1.,0.,0.));
#6645=DIRECTION('center_axis',(0.,-1.,0.));
#6646=DIRECTION('ref_axis',(1.,0.,0.));
#6647=DIRECTION('center_axis',(0.,-1.,0.));
#6648=DIRECTION('ref_axis',(1.,0.,0.));
#6649=DIRECTION('',(0.,1.,0.));
#6650=DIRECTION('center_axis',(0.,1.,0.));
#6651=DIRECTION('ref_axis',(1.,0.,0.));
#6652=DIRECTION('center_axis',(-0.618640030553172,0.,-0.785674558960115));
#6653=DIRECTION('ref_axis',(0.785674558960115,0.,-0.618640030553172));
#6654=DIRECTION('',(-0.785674558960115,0.,0.618640030553172));
#6655=DIRECTION('',(0.785674558960114,0.,-0.618640030553172));
#6656=DIRECTION('',(0.,-1.,0.));
#6657=DIRECTION('center_axis',(-0.871926239623235,0.,0.489637245985725));
#6658=DIRECTION('ref_axis',(-0.489637245985725,0.,-0.871926239623235));
#6659=DIRECTION('',(0.489637245985725,0.,0.871926239623235));
#6660=DIRECTION('',(-0.489637245985725,0.,-0.871926239623235));
#6661=DIRECTION('',(0.,-1.,0.));
#6662=DIRECTION('center_axis',(0.336992445886081,0.,0.941507350696593));
#6663=DIRECTION('ref_axis',(-0.941507350696593,0.,0.336992445886081));
#6664=DIRECTION('',(0.941507350696593,0.,-0.336992445886081));
#6665=DIRECTION('',(-0.941507350696593,0.,0.336992445886081));
#6666=DIRECTION('',(0.,-1.,0.));
#6667=DIRECTION('center_axis',(0.,-1.,0.));
#6668=DIRECTION('ref_axis',(1.,0.,0.));
#6669=DIRECTION('center_axis',(0.,-1.,0.));
#6670=DIRECTION('ref_axis',(1.,0.,0.));
#6671=DIRECTION('',(0.,1.,0.));
#6672=DIRECTION('center_axis',(0.,1.,0.));
#6673=DIRECTION('ref_axis',(1.,0.,0.));
#6674=DIRECTION('center_axis',(0.169919004238536,0.,-0.985458031576477));
#6675=DIRECTION('ref_axis',(0.985458031576477,0.,0.169919004238536));
#6676=DIRECTION('',(-0.985458031576477,0.,-0.169919004238536));
#6677=DIRECTION('',(0.985458031576477,0.,0.169919004238536));
#6678=DIRECTION('',(0.,-1.,0.));
#6679=DIRECTION('center_axis',(-0.947303919134588,0.,-0.32033620587166));
#6680=DIRECTION('ref_axis',(0.32033620587166,0.,-0.947303919134588));
#6681=DIRECTION('',(-0.32033620587166,0.,0.947303919134588));
#6682=DIRECTION('',(0.32033620587166,0.,-0.947303919134588));
#6683=DIRECTION('',(0.,-1.,0.));
#6684=DIRECTION('center_axis',(-0.474184356164995,0.,0.880425576848145));
#6685=DIRECTION('ref_axis',(-0.880425576848145,0.,-0.474184356164995));
#6686=DIRECTION('',(0.880425576848145,0.,0.474184356164995));
#6687=DIRECTION('',(-0.880425576848145,0.,-0.474184356164995));
#6688=DIRECTION('',(0.,-1.,0.));
#6689=DIRECTION('center_axis',(0.,-1.,0.));
#6690=DIRECTION('ref_axis',(1.,0.,0.));
#6691=DIRECTION('center_axis',(0.,-1.,0.));
#6692=DIRECTION('ref_axis',(1.,0.,0.));
#6693=DIRECTION('',(0.,1.,0.));
#6694=DIRECTION('center_axis',(0.,1.,0.));
#6695=DIRECTION('ref_axis',(1.,0.,0.));
#6696=DIRECTION('center_axis',(-0.962298216976301,0.,-0.271996583809855));
#6697=DIRECTION('ref_axis',(0.271996583809855,0.,-0.962298216976301));
#6698=DIRECTION('',(-0.271996583809855,0.,0.962298216976301));
#6699=DIRECTION('',(0.271996583809855,0.,-0.962298216976301));
#6700=DIRECTION('',(0.,-1.,0.));
#6701=DIRECTION('center_axis',(-0.417601593533129,0.,0.908630237818768));
#6702=DIRECTION('ref_axis',(-0.908630237818768,0.,-0.417601593533129));
#6703=DIRECTION('',(0.908630237818768,0.,0.417601593533129));
#6704=DIRECTION('',(-0.908630237818768,0.,-0.417601593533129));
#6705=DIRECTION('',(0.,-1.,0.));
#6706=DIRECTION('center_axis',(0.826036751362234,0.,0.563616257216669));
#6707=DIRECTION('ref_axis',(-0.563616257216669,0.,0.826036751362234));
#6708=DIRECTION('',(0.563616257216669,0.,-0.826036751362234));
#6709=DIRECTION('',(-0.563616257216669,0.,0.826036751362234));
#6710=DIRECTION('center_axis',(-0.768472187589368,0.,-0.639883190044567));
#6711=DIRECTION('ref_axis',(0.639883190044567,0.,-0.768472187589368));
#6712=DIRECTION('',(-0.639883190044567,0.,0.768472187589368));
#6713=DIRECTION('',(0.639883190044567,0.,-0.768472187589368));
#6714=DIRECTION('',(0.,-1.,0.));
#6715=DIRECTION('center_axis',(-0.751071251604073,0.,0.660221156139283));
#6716=DIRECTION('ref_axis',(-0.660221156139283,0.,-0.751071251604073));
#6717=DIRECTION('',(0.660221156139282,0.,0.751071251604074));
#6718=DIRECTION('',(-0.660221156139282,0.,-0.751071251604074));
#6719=DIRECTION('',(0.,-1.,0.));
#6720=DIRECTION('center_axis',(0.525378737609565,0.,0.850868486940126));
#6721=DIRECTION('ref_axis',(-0.850868486940126,0.,0.525378737609565));
#6722=DIRECTION('',(0.850868486940126,0.,-0.525378737609565));
#6723=DIRECTION('',(-0.850868486940126,0.,0.525378737609565));
#6724=DIRECTION('center_axis',(-0.0386823792600045,0.,-0.999251556683694));
#6725=DIRECTION('ref_axis',(0.999251556683694,0.,-0.0386823792600045));
#6726=DIRECTION('',(-0.999251556683694,0.,0.0386823792600045));
#6727=DIRECTION('',(0.999251556683694,0.,-0.0386823792600045));
#6728=DIRECTION('',(0.,-1.,0.));
#6729=DIRECTION('center_axis',(-0.993204697860151,0.,-0.116380531655973));
#6730=DIRECTION('ref_axis',(0.116380531655973,0.,-0.993204697860151));
#6731=DIRECTION('',(-0.116380531655973,0.,0.993204697860151));
#6732=DIRECTION('',(0.116380531655973,0.,-0.993204697860151));
#6733=DIRECTION('',(0.,-1.,0.));
#6734=DIRECTION('center_axis',(-0.280771519966595,0.,0.959774636868285));
#6735=DIRECTION('ref_axis',(-0.959774636868285,0.,-0.280771519966595));
#6736=DIRECTION('',(0.959774636868285,0.,0.280771519966595));
#6737=DIRECTION('',(-0.959774636868285,0.,-0.280771519966595));
#6738=DIRECTION('center_axis',(0.,0.,-1.));
#6739=DIRECTION('ref_axis',(1.,0.,0.));
#6740=DIRECTION('',(-1.,0.,0.));
#6741=DIRECTION('',(1.,0.,0.));
#6742=DIRECTION('center_axis',(0.,0.,1.));
#6743=DIRECTION('ref_axis',(-1.,0.,0.));
#6744=DIRECTION('',(1.,0.,0.));
#6745=DIRECTION('',(-1.,0.,0.));
#6746=DIRECTION('center_axis',(0.,-1.,0.));
#6747=DIRECTION('ref_axis',(1.,0.,0.));
#6748=DIRECTION('center_axis',(0.,-1.,0.));
#6749=DIRECTION('ref_axis',(1.,0.,0.));
#6750=DIRECTION('',(0.,-1.,0.));
#6751=DIRECTION('center_axis',(0.,1.,0.));
#6752=DIRECTION('ref_axis',(1.,0.,0.));
#6753=DIRECTION('center_axis',(0.,1.,0.));
#6754=DIRECTION('ref_axis',(1.,0.,0.));
#6755=DIRECTION('center_axis',(0.,1.,0.));
#6756=DIRECTION('ref_axis',(1.,0.,0.));
#6757=DIRECTION('axis',(0.,0.,1.));
#6758=DIRECTION('refdir',(1.,0.,0.));
#6759=DIRECTION('center_axis',(0.,-1.,0.));
#6760=DIRECTION('ref_axis',(1.,0.,0.));
#6761=DIRECTION('center_axis',(0.,-1.,0.));
#6762=DIRECTION('ref_axis',(1.,0.,0.));
#6763=DIRECTION('',(0.,-1.,0.));
#6764=DIRECTION('center_axis',(0.,1.,0.));
#6765=DIRECTION('ref_axis',(1.,0.,0.));
#6766=DIRECTION('center_axis',(1.,0.,0.));
#6767=DIRECTION('ref_axis',(0.,0.,-1.));
#6768=DIRECTION('',(0.,0.,1.));
#6769=DIRECTION('',(0.,1.,0.));
#6770=DIRECTION('',(0.,0.,-1.));
#6771=DIRECTION('',(0.,1.,0.));
#6772=DIRECTION('center_axis',(0.,0.,-1.));
#6773=DIRECTION('ref_axis',(-1.,0.,0.));
#6774=DIRECTION('',(1.,0.,0.));
#6775=DIRECTION('',(-1.,0.,0.));
#6776=DIRECTION('',(0.,1.,0.));
#6777=DIRECTION('center_axis',(1.,0.,0.));
#6778=DIRECTION('ref_axis',(0.,0.,-1.));
#6779=DIRECTION('',(0.,0.,1.));
#6780=DIRECTION('',(0.,0.,-1.));
#6781=DIRECTION('',(0.,1.,0.));
#6782=DIRECTION('center_axis',(0.,0.,1.));
#6783=DIRECTION('ref_axis',(1.,0.,0.));
#6784=DIRECTION('',(-1.,0.,0.));
#6785=DIRECTION('',(-1.,0.,0.));
#6786=DIRECTION('center_axis',(0.,1.,0.));
#6787=DIRECTION('ref_axis',(0.,0.,1.));
#6788=DIRECTION('center_axis',(0.,1.,0.));
#6789=DIRECTION('ref_axis',(1.,0.,0.));
#6790=DIRECTION('axis',(0.,0.,1.));
#6791=DIRECTION('refdir',(1.,0.,0.));
#6792=DIRECTION('center_axis',(-0.506446725163971,0.,-0.862271253475778));
#6793=DIRECTION('ref_axis',(-0.862271253475778,0.,0.506446725163971));
#6794=DIRECTION('',(0.862271253475778,0.,-0.506446725163971));
#6795=DIRECTION('',(0.,1.,0.));
#6796=DIRECTION('',(-0.862271253475778,0.,0.506446725163971));
#6797=DIRECTION('',(0.,-1.,0.));
#6798=DIRECTION('center_axis',(0.514130343945888,0.,-0.857712066741563));
#6799=DIRECTION('ref_axis',(-0.857712066741563,0.,-0.514130343945888));
#6800=DIRECTION('',(-0.857712066741563,0.,-0.514130343945888));
#6801=DIRECTION('',(0.,-1.,0.));
#6802=DIRECTION('',(-0.857712066741563,0.,-0.514130343945888));
#6803=DIRECTION('',(0.,1.,0.));
#6804=DIRECTION('center_axis',(0.,1.,0.));
#6805=DIRECTION('ref_axis',(-0.65291015697706,0.,-0.757435361543274));
#6806=DIRECTION('center_axis',(0.,-1.,0.));
#6807=DIRECTION('ref_axis',(-0.65291015697706,0.,-0.757435361543274));
#6808=DIRECTION('center_axis',(0.,1.,0.));
#6809=DIRECTION('ref_axis',(-0.65291015697706,0.,-0.757435361543274));
#6810=DIRECTION('center_axis',(0.692652702068206,0.,0.72127126264507));
#6811=DIRECTION('ref_axis',(0.72127126264507,0.,-0.692652702068206));
#6812=DIRECTION('',(0.72127126264507,0.,-0.692652702068206));
#6813=DIRECTION('',(0.,-1.,0.));
#6814=DIRECTION('',(0.72127126264507,0.,-0.692652702068206));
#6815=DIRECTION('',(0.,1.,0.));
#6816=DIRECTION('center_axis',(-0.684689477581543,0.,0.728834905372345));
#6817=DIRECTION('ref_axis',(0.728834905372345,0.,0.684689477581543));
#6818=DIRECTION('',(-0.728834905372345,0.,-0.684689477581542));
#6819=DIRECTION('',(0.728834905372345,0.,0.684689477581542));
#6820=DIRECTION('',(0.,-1.,0.));
#6821=DIRECTION('center_axis',(0.,-1.,0.));
#6822=DIRECTION('ref_axis',(1.,0.,0.));
#6823=DIRECTION('center_axis',(0.,-1.,0.));
#6824=DIRECTION('ref_axis',(1.,0.,0.));
#6825=DIRECTION('',(0.,-1.,0.));
#6826=DIRECTION('center_axis',(0.,1.,0.));
#6827=DIRECTION('ref_axis',(1.,0.,0.));
#6828=DIRECTION('center_axis',(0.685364699004991,0.,-0.728199992692803));
#6829=DIRECTION('ref_axis',(0.728199992692803,0.,0.685364699004991));
#6830=DIRECTION('',(-0.728199992692803,0.,-0.685364699004991));
#6831=DIRECTION('',(0.728199992692803,0.,0.685364699004991));
#6832=DIRECTION('',(0.,-1.,0.));
#6833=DIRECTION('center_axis',(0.,-1.,0.));
#6834=DIRECTION('ref_axis',(-0.922431509667951,0.,-0.38616073074784));
#6835=DIRECTION('center_axis',(0.,1.,0.));
#6836=DIRECTION('ref_axis',(-0.922431509667951,0.,-0.38616073074784));
#6837=DIRECTION('center_axis',(0.,-1.,0.));
#6838=DIRECTION('ref_axis',(-0.922431509667951,0.,-0.38616073074784));
#6839=DIRECTION('center_axis',(0.752564828001213,0.,0.658518169571277));
#6840=DIRECTION('ref_axis',(-0.658518169571277,0.,0.752564828001213));
#6841=DIRECTION('',(0.658518169571277,0.,-0.752564828001213));
#6842=DIRECTION('',(-0.658518169571277,0.,0.752564828001213));
#6843=DIRECTION('',(0.,-1.,0.));
#6844=DIRECTION('center_axis',(0.,-1.,0.));
#6845=DIRECTION('ref_axis',(0.321121156101037,0.,-0.947038121251903));
#6846=DIRECTION('center_axis',(0.,1.,0.));
#6847=DIRECTION('ref_axis',(0.321121156101037,0.,-0.947038121251903));
#6848=DIRECTION('center_axis',(0.,-1.,0.));
#6849=DIRECTION('ref_axis',(0.321121156101037,0.,-0.947038121251903));
#6850=DIRECTION('center_axis',(0.,1.,0.));
#6851=DIRECTION('ref_axis',(1.,0.,0.));
#6852=DIRECTION('center_axis',(0.,1.,0.));
#6853=DIRECTION('ref_axis',(1.,0.,0.));
#6854=DIRECTION('axis',(0.,0.,1.));
#6855=DIRECTION('refdir',(1.,0.,0.));
#6856=DIRECTION('center_axis',(0.,1.,0.));
#6857=DIRECTION('ref_axis',(1.,0.,0.));
#6858=DIRECTION('center_axis',(0.,-1.,0.));
#6859=DIRECTION('ref_axis',(1.,0.,0.));
#6860=DIRECTION('',(0.,-1.,0.));
#6861=DIRECTION('center_axis',(0.,-1.,0.));
#6862=DIRECTION('ref_axis',(1.,0.,0.));
#6863=DIRECTION('center_axis',(0.,1.,0.));
#6864=DIRECTION('ref_axis',(1.,0.,0.));
#6865=DIRECTION('center_axis',(0.,1.,0.));
#6866=DIRECTION('ref_axis',(0.,0.,1.));
#6867=DIRECTION('axis',(0.,0.,1.));
#6868=DIRECTION('refdir',(1.,0.,0.));
#6869=DIRECTION('center_axis',(0.,-1.,0.));
#6870=DIRECTION('ref_axis',(1.,0.,0.));
#6871=DIRECTION('center_axis',(0.,-1.,0.));
#6872=DIRECTION('ref_axis',(1.,0.,0.));
#6873=DIRECTION('center_axis',(0.,-1.,0.));
#6874=DIRECTION('ref_axis',(1.,0.,0.));
#6875=DIRECTION('center_axis',(0.,0.,-1.));
#6876=DIRECTION('ref_axis',(0.,1.,0.));
#6877=DIRECTION('',(1.,0.,0.));
#6878=DIRECTION('',(-1.,0.,0.));
#6879=DIRECTION('center_axis',(0.,1.,0.));
#6880=DIRECTION('ref_axis',(0.,0.,1.));
#6881=DIRECTION('center_axis',(0.,1.,0.));
#6882=DIRECTION('ref_axis',(0.,0.,-1.));
#6883=DIRECTION('',(-1.,0.,0.));
#6884=DIRECTION('center_axis',(0.,1.,0.));
#6885=DIRECTION('ref_axis',(0.,0.,-1.));
#6886=DIRECTION('center_axis',(0.,1.,0.));
#6887=DIRECTION('ref_axis',(0.,0.,-1.));
#6888=DIRECTION('center_axis',(0.,0.,1.));
#6889=DIRECTION('ref_axis',(0.,-1.,0.));
#6890=DIRECTION('',(1.,0.,0.));
#6891=DIRECTION('center_axis',(0.,-1.,0.));
#6892=DIRECTION('ref_axis',(1.,0.,0.));
#6893=DIRECTION('center_axis',(0.,1.,0.));
#6894=DIRECTION('ref_axis',(-1.,0.,0.));
#6895=DIRECTION('center_axis',(0.,-1.,0.));
#6896=DIRECTION('ref_axis',(-1.,0.,0.));
#6897=DIRECTION('center_axis',(0.,0.,1.));
#6898=DIRECTION('ref_axis',(1.,0.,0.));
#6899=DIRECTION('center_axis',(0.,1.,0.));
#6900=DIRECTION('ref_axis',(-1.,0.,0.));
#6901=DIRECTION('center_axis',(0.,-1.,0.));
#6902=DIRECTION('ref_axis',(1.,0.,0.));
#6903=DIRECTION('center_axis',(0.,-1.,0.));
#6904=DIRECTION('ref_axis',(1.,0.,0.));
#6905=DIRECTION('center_axis',(0.,1.,0.));
#6906=DIRECTION('ref_axis',(1.,0.,0.));
#6907=DIRECTION('center_axis',(0.,-1.,0.));
#6908=DIRECTION('ref_axis',(1.,0.,0.));
#6909=DIRECTION('',(0.,1.,0.));
#6910=DIRECTION('axis',(0.,0.,1.));
#6911=DIRECTION('refdir',(1.,0.,0.));
#6912=DIRECTION('center_axis',(0.,-1.,0.));
#6913=DIRECTION('ref_axis',(1.,0.,0.));
#6914=DIRECTION('center_axis',(0.,-1.,0.));
#6915=DIRECTION('ref_axis',(1.,0.,0.));
#6916=DIRECTION('',(0.,1.,0.));
#6917=DIRECTION('center_axis',(0.,-1.,0.));
#6918=DIRECTION('ref_axis',(1.,0.,0.));
#6919=DIRECTION('center_axis',(0.,-1.,0.));
#6920=DIRECTION('ref_axis',(1.,0.,0.));
#6921=DIRECTION('center_axis',(0.,-1.,0.));
#6922=DIRECTION('ref_axis',(1.,0.,0.));
#6923=DIRECTION('axis',(0.,0.,1.));
#6924=DIRECTION('refdir',(1.,0.,0.));
#6925=DIRECTION('center_axis',(-1.,-1.83697019872103E-16,0.));
#6926=DIRECTION('ref_axis',(1.83697019872103E-16,-1.,0.));
#6927=DIRECTION('center_axis',(-1.,-1.83697019872103E-16,0.));
#6928=DIRECTION('ref_axis',(1.83697019872103E-16,-1.,0.));
#6929=DIRECTION('',(-1.,-1.83697019872103E-16,0.));
#6930=DIRECTION('center_axis',(-1.,-1.83697019872103E-16,0.));
#6931=DIRECTION('ref_axis',(1.83697019872103E-16,-1.,0.));
#6932=DIRECTION('center_axis',(-1.,-1.83697019872103E-16,0.));
#6933=DIRECTION('ref_axis',(1.83697019872103E-16,-1.,0.));
#6934=DIRECTION('center_axis',(-1.,-1.83697019872103E-16,0.));
#6935=DIRECTION('ref_axis',(1.83697019872103E-16,-1.,0.));
#6936=DIRECTION('',(-1.,-1.83697019872103E-16,0.));
#6937=DIRECTION('center_axis',(-1.,-1.83697019872103E-16,0.));
#6938=DIRECTION('ref_axis',(1.83697019872103E-16,-1.,0.));
#6939=DIRECTION('center_axis',(-1.,-1.83697019872103E-16,0.));
#6940=DIRECTION('ref_axis',(1.83697019872103E-16,-1.,0.));
#6941=DIRECTION('center_axis',(-1.,-1.83697019872103E-16,0.));
#6942=DIRECTION('ref_axis',(1.83697019872103E-16,-1.,0.));
#6943=DIRECTION('center_axis',(-1.,-1.83697019872103E-16,0.));
#6944=DIRECTION('ref_axis',(1.83697019872103E-16,-1.,0.));
#6945=DIRECTION('',(-1.,-1.83697019872103E-16,0.));
#6946=DIRECTION('center_axis',(-1.,-1.83697019872103E-16,0.));
#6947=DIRECTION('ref_axis',(1.83697019872103E-16,-1.,0.));
#6948=DIRECTION('center_axis',(1.,1.83697019872103E-16,0.));
#6949=DIRECTION('ref_axis',(-1.83697019872103E-16,1.,0.));
#6950=DIRECTION('',(0.707106781186551,-0.707106781186544,-8.6595605623549E-17));
#6951=DIRECTION('center_axis',(-1.,-1.83697019872103E-16,0.));
#6952=DIRECTION('ref_axis',(1.83697019872103E-16,-1.,0.));
#6953=DIRECTION('center_axis',(-1.,-1.83697019872103E-16,0.));
#6954=DIRECTION('ref_axis',(1.85037170770859E-16,-1.,0.));
#6955=DIRECTION('center_axis',(-1.,-1.83697019872103E-16,0.));
#6956=DIRECTION('ref_axis',(1.83697019872103E-16,-1.,0.));
#6957=DIRECTION('center_axis',(2.24963967399279E-32,-1.22464679914735E-16,
-1.));
#6958=DIRECTION('ref_axis',(-1.85037170770859E-16,1.,-1.22464679914735E-16));
#6959=DIRECTION('center_axis',(-1.,-1.83697019872103E-16,0.));
#6960=DIRECTION('ref_axis',(1.83697019872103E-16,-1.,0.));
#6961=DIRECTION('center_axis',(-1.,-1.83697019872103E-16,0.));
#6962=DIRECTION('ref_axis',(1.83697019872103E-16,-1.,0.));
#6963=DIRECTION('center_axis',(-1.,-1.83697019872103E-16,0.));
#6964=DIRECTION('ref_axis',(1.83697019872103E-16,-1.,0.));
#6965=DIRECTION('',(1.,1.83697019872103E-16,0.));
#6966=DIRECTION('center_axis',(-1.,-1.83697019872103E-16,0.));
#6967=DIRECTION('ref_axis',(1.85037170770859E-16,-1.,0.));
#6968=DIRECTION('center_axis',(-1.,-1.83697019872103E-16,0.));
#6969=DIRECTION('ref_axis',(1.83697019872103E-16,-1.,0.));
#6970=DIRECTION('center_axis',(2.24963967399279E-32,-1.22464679914735E-16,
-1.));
#6971=DIRECTION('ref_axis',(-1.85037170770859E-16,1.,-1.22464679914735E-16));
#6972=DIRECTION('center_axis',(-1.,-1.83697019872103E-16,0.));
#6973=DIRECTION('ref_axis',(1.83697019872103E-16,-1.,0.));
#6974=DIRECTION('',(-0.707106781186551,0.707106781186544,-8.6595605623549E-17));
#6975=DIRECTION('center_axis',(-1.,-1.83697019872103E-16,0.));
#6976=DIRECTION('ref_axis',(1.83697019872103E-16,-1.,0.));
#6977=DIRECTION('center_axis',(1.,1.83697019872103E-16,0.));
#6978=DIRECTION('ref_axis',(-1.83697019872103E-16,1.,0.));
#6979=DIRECTION('center_axis',(-1.,-1.83697019872103E-16,0.));
#6980=DIRECTION('ref_axis',(1.83697019872103E-16,-1.,0.));
#6981=DIRECTION('center_axis',(1.,1.83697019872103E-16,0.));
#6982=DIRECTION('ref_axis',(-1.83697019872103E-16,1.,0.));
#6983=DIRECTION('center_axis',(-1.,-1.83697019872103E-16,0.));
#6984=DIRECTION('ref_axis',(1.83697019872103E-16,-1.,0.));
#6985=DIRECTION('center_axis',(1.,1.83697019872103E-16,0.));
#6986=DIRECTION('ref_axis',(-1.83697019872103E-16,1.,0.));
#6987=DIRECTION('center_axis',(-1.,-1.83697019872103E-16,0.));
#6988=DIRECTION('ref_axis',(1.83697019872103E-16,-1.,0.));
#6989=DIRECTION('',(-0.707106781186548,0.707106781186547,8.65956056235493E-17));
#6990=DIRECTION('center_axis',(-1.,-1.83697019872103E-16,0.));
#6991=DIRECTION('ref_axis',(1.83697019872103E-16,-1.,0.));
#6992=DIRECTION('center_axis',(-1.,-1.83697019872103E-16,0.));
#6993=DIRECTION('ref_axis',(1.83697019872103E-16,-1.,0.));
#6994=DIRECTION('center_axis',(-1.,-1.83697019872103E-16,0.));
#6995=DIRECTION('ref_axis',(1.83697019872103E-16,-1.,0.));
#6996=DIRECTION('',(1.,1.83697019872103E-16,0.));
#6997=DIRECTION('center_axis',(-1.,-1.83697019872103E-16,0.));
#6998=DIRECTION('ref_axis',(1.83697019872103E-16,-1.,0.));
#6999=DIRECTION('center_axis',(-1.,-1.83697019872103E-16,0.));
#7000=DIRECTION('ref_axis',(1.96129949112834E-16,-1.,0.));
#7001=DIRECTION('center_axis',(-2.24963967399279E-32,1.22464679914735E-16,
1.));
#7002=DIRECTION('ref_axis',(-1.63441624260695E-16,1.,-1.22464679914735E-16));
#7003=DIRECTION('center_axis',(-1.,-1.83697019872103E-16,0.));
#7004=DIRECTION('ref_axis',(1.83697019872103E-16,-1.,0.));
#7005=DIRECTION('center_axis',(-1.,-1.83697019872103E-16,0.));
#7006=DIRECTION('ref_axis',(1.83697019872103E-16,-1.,0.));
#7007=DIRECTION('center_axis',(-1.,-1.83697019872103E-16,0.));
#7008=DIRECTION('ref_axis',(1.83697019872103E-16,-1.,0.));
#7009=DIRECTION('',(1.,1.83697019872103E-16,0.));
#7010=DIRECTION('center_axis',(-1.,-1.83697019872103E-16,0.));
#7011=DIRECTION('ref_axis',(1.83697019872103E-16,-1.,0.));
#7012=DIRECTION('center_axis',(-1.,-1.83697019872103E-16,0.));
#7013=DIRECTION('ref_axis',(1.96129949112834E-16,-1.,0.));
#7014=DIRECTION('center_axis',(-1.,-1.83697019872103E-16,0.));
#7015=DIRECTION('ref_axis',(1.83697019872103E-16,-1.,0.));
#7016=DIRECTION('center_axis',(-2.24963967399279E-32,1.22464679914735E-16,
1.));
#7017=DIRECTION('ref_axis',(-1.63441624260695E-16,1.,-1.22464679914735E-16));
#7018=DIRECTION('center_axis',(-1.,-1.83697019872103E-16,0.));
#7019=DIRECTION('ref_axis',(1.83697019872103E-16,-1.,0.));
#7020=DIRECTION('center_axis',(-1.,-1.83697019872103E-16,0.));
#7021=DIRECTION('ref_axis',(1.83697019872103E-16,-1.,0.));
#7022=DIRECTION('',(1.,1.83697019872103E-16,0.));
#7023=DIRECTION('center_axis',(-1.,-1.83697019872103E-16,0.));
#7024=DIRECTION('ref_axis',(1.83697019872103E-16,-1.,0.));
#7025=DIRECTION('center_axis',(-1.,-1.83697019872103E-16,0.));
#7026=DIRECTION('ref_axis',(1.83697019872103E-16,-1.,0.));
#7027=DIRECTION('',(0.707106781186548,-0.707106781186547,8.65956056235493E-17));
#7028=DIRECTION('center_axis',(-1.,-1.83697019872103E-16,0.));
#7029=DIRECTION('ref_axis',(1.83697019872103E-16,-1.,0.));
#7030=DIRECTION('center_axis',(-1.,-1.83697019872103E-16,0.));
#7031=DIRECTION('ref_axis',(1.85037170770859E-16,-1.,0.));
#7032=DIRECTION('center_axis',(-1.,-1.83697019872103E-16,0.));
#7033=DIRECTION('ref_axis',(1.83697019872103E-16,-1.,0.));
#7034=DIRECTION('center_axis',(2.24963967399279E-32,-1.22464679914735E-16,
-1.));
#7035=DIRECTION('ref_axis',(-2.31296463463574E-16,1.,-1.22464679914735E-16));
#7036=DIRECTION('center_axis',(-1.,-1.83697019872103E-16,0.));
#7037=DIRECTION('ref_axis',(1.83697019872103E-16,-1.,0.));
#7038=DIRECTION('center_axis',(-1.,-1.83697019872103E-16,0.));
#7039=DIRECTION('ref_axis',(1.83697019872103E-16,-1.,0.));
#7040=DIRECTION('',(-1.,-1.83697019872103E-16,0.));
#7041=DIRECTION('center_axis',(-1.,-1.83697019872103E-16,0.));
#7042=DIRECTION('ref_axis',(1.83697019872103E-16,-1.,0.));
#7043=DIRECTION('center_axis',(-1.,-1.83697019872103E-16,0.));
#7044=DIRECTION('ref_axis',(1.85037170770859E-16,-1.,0.));
#7045=DIRECTION('center_axis',(2.24963967399279E-32,-1.22464679914735E-16,
-1.));
#7046=DIRECTION('ref_axis',(-2.31296463463574E-16,1.,-1.22464679914735E-16));
#7047=DIRECTION('center_axis',(-1.,-1.83697019872103E-16,0.));
#7048=DIRECTION('ref_axis',(1.83697019872103E-16,-1.,0.));
#7049=DIRECTION('center_axis',(-1.,-1.83697019872103E-16,0.));
#7050=DIRECTION('ref_axis',(1.83697019872103E-16,-1.,0.));
#7051=DIRECTION('center_axis',(-1.,-1.83697019872103E-16,0.));
#7052=DIRECTION('ref_axis',(1.83697019872103E-16,-1.,0.));
#7053=DIRECTION('center_axis',(1.,1.83697019872103E-16,0.));
#7054=DIRECTION('ref_axis',(-1.83697019872103E-16,1.,0.));
#7055=DIRECTION('center_axis',(1.,1.83697019872103E-16,0.));
#7056=DIRECTION('ref_axis',(-1.83697019872103E-16,1.,0.));
#7057=DIRECTION('center_axis',(-1.,-1.83697019872103E-16,0.));
#7058=DIRECTION('ref_axis',(1.83697019872103E-16,-1.,0.));
#7059=DIRECTION('center_axis',(-1.,-1.83697019872103E-16,0.));
#7060=DIRECTION('ref_axis',(1.83697019872103E-16,-1.,0.));
#7061=DIRECTION('',(-1.,-1.83697019872103E-16,0.));
#7062=DIRECTION('center_axis',(-1.,-1.83697019872103E-16,0.));
#7063=DIRECTION('ref_axis',(1.83697019872103E-16,-1.,0.));
#7064=DIRECTION('center_axis',(-1.,-1.83697019872103E-16,0.));
#7065=DIRECTION('ref_axis',(1.57361694361665E-16,-1.,0.));
#7066=DIRECTION('center_axis',(-1.,-1.83697019872103E-16,0.));
#7067=DIRECTION('ref_axis',(1.83697019872103E-16,-1.,0.));
#7068=DIRECTION('center_axis',(2.24963967399279E-32,-1.22464679914735E-16,
-1.));
#7069=DIRECTION('ref_axis',(-1.96702117952081E-16,1.,-1.22464679914735E-16));
#7070=DIRECTION('center_axis',(-1.,-1.83697019872103E-16,0.));
#7071=DIRECTION('ref_axis',(1.83697019872103E-16,-1.,0.));
#7072=DIRECTION('center_axis',(-1.,-1.83697019872103E-16,0.));
#7073=DIRECTION('ref_axis',(1.83697019872103E-16,-1.,0.));
#7074=DIRECTION('center_axis',(-1.,-1.83697019872103E-16,0.));
#7075=DIRECTION('ref_axis',(1.83697019872103E-16,-1.,0.));
#7076=DIRECTION('',(0.866025403784443,-0.499999999999992,6.12323399573667E-17));
#7077=DIRECTION('center_axis',(-1.,-1.83697019872103E-16,0.));
#7078=DIRECTION('ref_axis',(2.01689087919369E-16,-1.,0.));
#7079=DIRECTION('center_axis',(-1.,-1.83697019872103E-16,0.));
#7080=DIRECTION('ref_axis',(1.83697019872103E-16,-1.,0.));
#7081=DIRECTION('center_axis',(-2.24963967399279E-32,1.22464679914735E-16,
1.));
#7082=DIRECTION('ref_axis',(-1.89083519924408E-16,1.,-1.22464679914735E-16));
#7083=DIRECTION('center_axis',(-1.,-1.83697019872103E-16,0.));
#7084=DIRECTION('ref_axis',(1.88974131851091E-16,-1.,0.));
#7085=DIRECTION('center_axis',(-1.,-1.83697019872103E-16,0.));
#7086=DIRECTION('ref_axis',(1.83697019872103E-16,-1.,0.));
#7087=DIRECTION('center_axis',(-2.24963967399279E-32,1.22464679914735E-16,
1.));
#7088=DIRECTION('ref_axis',(-1.77163248610397E-16,1.,-1.22464679914735E-16));
#7089=DIRECTION('center_axis',(-1.,-1.83697019872103E-16,0.));
#7090=DIRECTION('ref_axis',(1.83697019872103E-16,-1.,0.));
#7091=DIRECTION('center_axis',(-1.,-1.83697019872103E-16,0.));
#7092=DIRECTION('ref_axis',(1.83697019872103E-16,-1.,0.));
#7093=DIRECTION('center_axis',(-1.,-1.83697019872103E-16,0.));
#7094=DIRECTION('ref_axis',(1.83697019872103E-16,-1.,0.));
#7095=DIRECTION('',(-0.500000000000007,0.866025403784435,-1.0605752387249E-16));
#7096=DIRECTION('center_axis',(-1.,-1.83697019872103E-16,0.));
#7097=DIRECTION('ref_axis',(1.91801449774277E-16,-1.,0.));
#7098=DIRECTION('center_axis',(-1.,-1.83697019872103E-16,0.));
#7099=DIRECTION('ref_axis',(1.83697019872103E-16,-1.,0.));
#7100=DIRECTION('center_axis',(-2.24963967399279E-32,1.22464679914735E-16,
1.));
#7101=DIRECTION('ref_axis',(-1.79813859163385E-16,1.,-1.22464679914735E-16));
#7102=DIRECTION('center_axis',(-1.,-1.83697019872103E-16,0.));
#7103=DIRECTION('ref_axis',(1.87747066251861E-16,-1.,0.));
#7104=DIRECTION('center_axis',(-1.,-1.83697019872103E-16,0.));
#7105=DIRECTION('ref_axis',(1.83697019872103E-16,-1.,0.));
#7106=DIRECTION('center_axis',(2.24963967399279E-32,-1.22464679914735E-16,
-1.));
#7107=DIRECTION('ref_axis',(-1.7601287461112E-16,1.,-1.22464679914735E-16));
#7108=DIRECTION('center_axis',(-1.,-1.83697019872103E-16,0.));
#7109=DIRECTION('ref_axis',(1.83697019872103E-16,-1.,0.));
#7110=DIRECTION('center_axis',(-1.,-1.83697019872103E-16,0.));
#7111=DIRECTION('ref_axis',(1.83697019872103E-16,-1.,0.));
#7112=DIRECTION('center_axis',(-1.,-1.83697019872103E-16,0.));
#7113=DIRECTION('ref_axis',(1.83697019872103E-16,-1.,0.));
#7114=DIRECTION('',(0.500000000000007,-0.866025403784435,1.0605752387249E-16));
#7115=DIRECTION('center_axis',(-1.,-1.83697019872103E-16,0.));
#7116=DIRECTION('ref_axis',(1.85037170770859E-16,-1.,0.));
#7117=DIRECTION('center_axis',(-1.,-1.83697019872103E-16,0.));
#7118=DIRECTION('ref_axis',(1.83697019872103E-16,-1.,0.));
#7119=DIRECTION('center_axis',(2.24963967399279E-32,-1.22464679914735E-16,
-1.));
#7120=DIRECTION('ref_axis',(-1.73472347597681E-16,1.,-1.22464679914735E-16));
#7121=DIRECTION('center_axis',(-1.,-1.83697019872103E-16,0.));
#7122=DIRECTION('ref_axis',(1.97210791246963E-16,-1.,0.));
#7123=DIRECTION('center_axis',(-1.,-1.83697019872103E-16,0.));
#7124=DIRECTION('ref_axis',(1.83697019872103E-16,-1.,0.));
#7125=DIRECTION('center_axis',(2.24963967399279E-32,-1.22464679914735E-16,
-1.));
#7126=DIRECTION('ref_axis',(-1.84885116794028E-16,1.,-1.22464679914735E-16));
#7127=DIRECTION('center_axis',(-1.,-1.83697019872103E-16,0.));
#7128=DIRECTION('ref_axis',(1.83697019872103E-16,-1.,0.));
#7129=DIRECTION('center_axis',(-1.,-1.83697019872103E-16,0.));
#7130=DIRECTION('ref_axis',(1.83697019872103E-16,-1.,0.));
#7131=DIRECTION('center_axis',(-1.,-1.83697019872103E-16,0.));
#7132=DIRECTION('ref_axis',(1.83697019872103E-16,-1.,0.));
#7133=DIRECTION('',(-0.866025403784443,0.499999999999992,-6.12323399573667E-17));
#7134=DIRECTION('center_axis',(1.,1.83697019872103E-16,0.));
#7135=DIRECTION('ref_axis',(-1.83697019872103E-16,1.,0.));
#7136=DIRECTION('center_axis',(1.,1.83697019872103E-16,0.));
#7137=DIRECTION('ref_axis',(-1.83697019872103E-16,1.,0.));
#7138=DIRECTION('center_axis',(-1.,-1.83697019872103E-16,0.));
#7139=DIRECTION('ref_axis',(1.83697019872103E-16,-1.,0.));
#7140=DIRECTION('center_axis',(1.,1.83697019872103E-16,0.));
#7141=DIRECTION('ref_axis',(-1.83697019872103E-16,1.,0.));
#7142=DIRECTION('center_axis',(1.,1.83697019872103E-16,0.));
#7143=DIRECTION('ref_axis',(-1.83697019872103E-16,1.,0.));
#7144=DIRECTION('center_axis',(1.,-1.83697019872103E-16,0.));
#7145=DIRECTION('ref_axis',(-1.83697019872103E-16,-1.,0.));
#7146=DIRECTION('center_axis',(-1.,1.83697019872103E-16,0.));
#7147=DIRECTION('ref_axis',(-1.83697019872103E-16,-1.,0.));
#7148=DIRECTION('',(1.,-1.83697019872103E-16,0.));
#7149=DIRECTION('center_axis',(-1.,1.83697019872103E-16,0.));
#7150=DIRECTION('ref_axis',(-1.83697019872103E-16,-1.,0.));
#7151=DIRECTION('center_axis',(1.,-1.83697019872103E-16,0.));
#7152=DIRECTION('ref_axis',(-1.57361694361665E-16,-1.,0.));
#7153=DIRECTION('center_axis',(-1.,1.83697019872103E-16,0.));
#7154=DIRECTION('ref_axis',(-1.83697019872103E-16,-1.,0.));
#7155=DIRECTION('center_axis',(-2.24963967399279E-32,-1.22464679914735E-16,
1.));
#7156=DIRECTION('ref_axis',(1.96702117952081E-16,1.,1.22464679914735E-16));
#7157=DIRECTION('center_axis',(-1.,1.83697019872103E-16,0.));
#7158=DIRECTION('ref_axis',(-1.83697019872103E-16,-1.,0.));
#7159=DIRECTION('center_axis',(1.,-1.83697019872103E-16,0.));
#7160=DIRECTION('ref_axis',(-1.83697019872103E-16,-1.,0.));
#7161=DIRECTION('center_axis',(-1.,1.83697019872103E-16,0.));
#7162=DIRECTION('ref_axis',(-1.83697019872103E-16,-1.,0.));
#7163=DIRECTION('',(-0.866025403784443,-0.499999999999992,-6.12323399573667E-17));
#7164=DIRECTION('center_axis',(1.,-1.83697019872103E-16,0.));
#7165=DIRECTION('ref_axis',(-2.01689087919369E-16,-1.,0.));
#7166=DIRECTION('center_axis',(-1.,1.83697019872103E-16,0.));
#7167=DIRECTION('ref_axis',(-1.83697019872103E-16,-1.,0.));
#7168=DIRECTION('center_axis',(2.24963967399279E-32,1.22464679914735E-16,
-1.));
#7169=DIRECTION('ref_axis',(1.89083519924408E-16,1.,1.22464679914735E-16));
#7170=DIRECTION('center_axis',(1.,-1.83697019872103E-16,0.));
#7171=DIRECTION('ref_axis',(-1.88974131851091E-16,-1.,0.));
#7172=DIRECTION('center_axis',(-1.,1.83697019872103E-16,0.));
#7173=DIRECTION('ref_axis',(-1.83697019872103E-16,-1.,0.));
#7174=DIRECTION('center_axis',(2.24963967399279E-32,1.22464679914735E-16,
-1.));
#7175=DIRECTION('ref_axis',(1.77163248610397E-16,1.,1.22464679914735E-16));
#7176=DIRECTION('center_axis',(-1.,1.83697019872103E-16,0.));
#7177=DIRECTION('ref_axis',(-1.83697019872103E-16,-1.,0.));
#7178=DIRECTION('center_axis',(1.,-1.83697019872103E-16,0.));
#7179=DIRECTION('ref_axis',(-1.83697019872103E-16,-1.,0.));
#7180=DIRECTION('center_axis',(-1.,1.83697019872103E-16,0.));
#7181=DIRECTION('ref_axis',(-1.83697019872103E-16,-1.,0.));
#7182=DIRECTION('',(0.500000000000007,0.866025403784435,1.0605752387249E-16));
#7183=DIRECTION('center_axis',(1.,-1.83697019872103E-16,0.));
#7184=DIRECTION('ref_axis',(-1.91801449774277E-16,-1.,0.));
#7185=DIRECTION('center_axis',(-1.,1.83697019872103E-16,0.));
#7186=DIRECTION('ref_axis',(-1.83697019872103E-16,-1.,0.));
#7187=DIRECTION('center_axis',(2.24963967399279E-32,1.22464679914735E-16,
-1.));
#7188=DIRECTION('ref_axis',(1.79813859163385E-16,1.,1.22464679914735E-16));
#7189=DIRECTION('center_axis',(1.,-1.83697019872103E-16,0.));
#7190=DIRECTION('ref_axis',(-1.87747066251861E-16,-1.,0.));
#7191=DIRECTION('center_axis',(-1.,1.83697019872103E-16,0.));
#7192=DIRECTION('ref_axis',(-1.83697019872103E-16,-1.,0.));
#7193=DIRECTION('center_axis',(-2.24963967399279E-32,-1.22464679914735E-16,
1.));
#7194=DIRECTION('ref_axis',(1.7601287461112E-16,1.,1.22464679914735E-16));
#7195=DIRECTION('center_axis',(-1.,1.83697019872103E-16,0.));
#7196=DIRECTION('ref_axis',(-1.83697019872103E-16,-1.,0.));
#7197=DIRECTION('center_axis',(1.,-1.83697019872103E-16,0.));
#7198=DIRECTION('ref_axis',(-1.83697019872103E-16,-1.,0.));
#7199=DIRECTION('center_axis',(-1.,1.83697019872103E-16,0.));
#7200=DIRECTION('ref_axis',(-1.83697019872103E-16,-1.,0.));
#7201=DIRECTION('',(-0.500000000000007,-0.866025403784435,-1.0605752387249E-16));
#7202=DIRECTION('center_axis',(1.,-1.83697019872103E-16,0.));
#7203=DIRECTION('ref_axis',(-1.85037170770859E-16,-1.,0.));
#7204=DIRECTION('center_axis',(-1.,1.83697019872103E-16,0.));
#7205=DIRECTION('ref_axis',(-1.83697019872103E-16,-1.,0.));
#7206=DIRECTION('center_axis',(-2.24963967399279E-32,-1.22464679914735E-16,
1.));
#7207=DIRECTION('ref_axis',(1.73472347597681E-16,1.,1.22464679914735E-16));
#7208=DIRECTION('center_axis',(1.,-1.83697019872103E-16,0.));
#7209=DIRECTION('ref_axis',(-1.97210791246963E-16,-1.,0.));
#7210=DIRECTION('center_axis',(-1.,1.83697019872103E-16,0.));
#7211=DIRECTION('ref_axis',(-1.83697019872103E-16,-1.,0.));
#7212=DIRECTION('center_axis',(-2.24963967399279E-32,-1.22464679914735E-16,
1.));
#7213=DIRECTION('ref_axis',(1.84885116794028E-16,1.,1.22464679914735E-16));
#7214=DIRECTION('center_axis',(-1.,1.83697019872103E-16,0.));
#7215=DIRECTION('ref_axis',(-1.83697019872103E-16,-1.,0.));
#7216=DIRECTION('center_axis',(1.,-1.83697019872103E-16,0.));
#7217=DIRECTION('ref_axis',(-1.83697019872103E-16,-1.,0.));
#7218=DIRECTION('center_axis',(-1.,1.83697019872103E-16,0.));
#7219=DIRECTION('ref_axis',(-1.83697019872103E-16,-1.,0.));
#7220=DIRECTION('',(0.866025403784443,0.499999999999992,6.12323399573667E-17));
#7221=DIRECTION('center_axis',(-1.,1.83697019872103E-16,0.));
#7222=DIRECTION('ref_axis',(1.83697019872103E-16,1.,0.));
#7223=DIRECTION('center_axis',(-1.,1.83697019872103E-16,0.));
#7224=DIRECTION('ref_axis',(1.83697019872103E-16,1.,0.));
#7225=DIRECTION('center_axis',(1.,-1.83697019872103E-16,0.));
#7226=DIRECTION('ref_axis',(-1.83697019872103E-16,-1.,0.));
#7227=DIRECTION('center_axis',(-1.,1.83697019872103E-16,0.));
#7228=DIRECTION('ref_axis',(1.83697019872103E-16,1.,0.));
#7229=DIRECTION('center_axis',(-1.,1.83697019872103E-16,0.));
#7230=DIRECTION('ref_axis',(1.83697019872103E-16,1.,0.));
#7231=DIRECTION('',(3.23556230657056E-32,1.23259516440783E-32,1.));
#7232=DIRECTION('',(-3.33066907387547E-16,1.,-1.23259516440783E-32));
#7233=DIRECTION('',(0.,0.,1.));
#7234=DIRECTION('',(1.,0.,0.));
#7235=DIRECTION('',(0.,0.,1.));
#7236=DIRECTION('',(1.,0.,0.));
#7237=DIRECTION('',(0.,0.,1.));
#7238=DIRECTION('',(1.,0.,0.));
#7239=DIRECTION('',(0.,0.,1.));
#7240=DIRECTION('',(1.,0.,0.));
#7241=DIRECTION('',(0.,0.,1.));
#7242=DIRECTION('',(1.,0.,0.));
#7243=DIRECTION('',(0.,0.,1.));
#7244=DIRECTION('',(1.,0.,0.));
#7245=DIRECTION('',(3.23556230657056E-32,1.3684555315672E-47,1.));
#7246=DIRECTION('',(-3.05311331771918E-16,1.,-4.10536659470161E-48));
#7247=CARTESIAN_POINT('',(0.,0.,0.));
#7248=CARTESIAN_POINT('',(0.,0.,0.));
#7249=CARTESIAN_POINT('Origin',(31.2735217236592,-4.5,50.3382969385033));
#7250=CARTESIAN_POINT('',(31.2735217236592,-2.5,50.3382969385033));
#7251=CARTESIAN_POINT('',(25.2794356395192,-2.5,49.3047581107688));
#7252=CARTESIAN_POINT('',(15.94574796428,-2.5,47.6953837235988));
#7253=CARTESIAN_POINT('',(25.2794356395192,-6.5,49.3047581107688));
#7254=CARTESIAN_POINT('',(25.2794356395192,-4.5,49.3047581107688));
#7255=CARTESIAN_POINT('',(31.2735217236592,-6.5,50.3382969385033));
#7256=CARTESIAN_POINT('',(31.5856264400152,-6.5,50.3921120386111));
#7257=CARTESIAN_POINT('',(31.2735217236592,-4.5,50.3382969385033));
#7258=CARTESIAN_POINT('Origin',(31.3062123347366,-4.5,50.2416236826399));
#7259=CARTESIAN_POINT('',(31.3062123347366,-2.5,50.2416236826399));
#7260=CARTESIAN_POINT('',(29.943512708519,-2.5,54.2714232271732));
#7261=CARTESIAN_POINT('',(31.3062123347366,-6.5,50.2416236826399));
#7262=CARTESIAN_POINT('',(31.0437587864934,-6.5,51.0177559782855));
#7263=CARTESIAN_POINT('',(31.3062123347366,-4.5,50.2416236826399));
#7264=CARTESIAN_POINT('Origin',(25.2333571880834,-4.5,46.9708726009778));
#7265=CARTESIAN_POINT('',(25.2333571880834,-2.5,46.9708726009778));
#7266=CARTESIAN_POINT('',(15.8012266428482,-2.5,41.8908648553283));
#7267=CARTESIAN_POINT('',(25.2333571880834,-6.5,46.9708726009778));
#7268=CARTESIAN_POINT('',(31.5856264400152,-6.5,50.3921120386111));
#7269=CARTESIAN_POINT('',(25.2333571880834,-4.5,46.9708726009778));
#7270=CARTESIAN_POINT('Origin',(0.,-4.5,48.6364583401654));
#7271=CARTESIAN_POINT('',(25.0282425392193,-2.5,52.2535796035455));
#7272=CARTESIAN_POINT('Origin',(0.,-2.5,48.6364583401654));
#7273=CARTESIAN_POINT('',(25.0282425392193,-6.5,52.2535796035455));
#7274=CARTESIAN_POINT('',(25.0282425392193,-4.5,52.2535796035455));
#7275=CARTESIAN_POINT('Origin',(0.,-6.5,48.6364583401654));
#7276=CARTESIAN_POINT('Origin',(0.,-4.5,48.6364583401654));
#7277=CARTESIAN_POINT('',(24.8659666539797,-6.5,44.0342639506209));
#7278=CARTESIAN_POINT('Origin',(0.,-6.5,48.6364583401654));
#7279=CARTESIAN_POINT('',(24.8659666539797,-2.5,44.0342639506209));
#7280=CARTESIAN_POINT('',(24.8659666539797,-4.5,44.0342639506209));
#7281=CARTESIAN_POINT('Origin',(0.,-2.5,48.6364583401654));
#7282=CARTESIAN_POINT('Origin',(26.3011261782795,-4.5,31.6311598314889));
#7283=CARTESIAN_POINT('',(26.3011261782795,-2.5,31.6311598314889));
#7284=CARTESIAN_POINT('',(20.8443097898499,-2.5,34.3182447567343));
#7285=CARTESIAN_POINT('',(12.3472313101976,-2.5,38.5024374922116));
#7286=CARTESIAN_POINT('',(20.8443097898499,-6.5,34.3182447567343));
#7287=CARTESIAN_POINT('',(20.8443097898499,-4.5,34.3182447567343));
#7288=CARTESIAN_POINT('',(26.3011261782795,-6.5,31.6311598314889));
#7289=CARTESIAN_POINT('',(26.5852559200301,-6.5,31.4912466125851));
#7290=CARTESIAN_POINT('',(26.3011261782795,-4.5,31.6311598314889));
#7291=CARTESIAN_POINT('Origin',(26.27075032411,-4.5,31.533734465514));
#7292=CARTESIAN_POINT('',(26.27075032411,-2.5,31.533734465514));
#7293=CARTESIAN_POINT('',(27.5369599102432,-2.5,35.5948855245611));
#7294=CARTESIAN_POINT('',(26.27075032411,-6.5,31.533734465514));
#7295=CARTESIAN_POINT('',(26.5146200605556,-6.5,32.3159050076438));
#7296=CARTESIAN_POINT('',(26.27075032411,-4.5,31.533734465514));
#7297=CARTESIAN_POINT('Origin',(19.4352080563696,-4.5,32.4571759505904));
#7298=CARTESIAN_POINT('',(19.4352080563695,-2.5,32.4571759505904));
#7299=CARTESIAN_POINT('',(8.81850051768697,-2.5,33.8914305849902));
#7300=CARTESIAN_POINT('',(19.4352080563696,-6.5,32.4571759505904));
#7301=CARTESIAN_POINT('',(26.5852559200301,-6.5,31.4912466125851));
#7302=CARTESIAN_POINT('',(19.4352080563695,-4.5,32.4571759505904));
#7303=CARTESIAN_POINT('Origin',(0.,-4.5,48.6364583401654));
#7304=CARTESIAN_POINT('',(22.3743640879347,-2.5,36.8515390576026));
#7305=CARTESIAN_POINT('Origin',(0.,-2.5,48.6364583401654));
#7306=CARTESIAN_POINT('',(22.3743640879347,-6.5,36.8515390576026));
#7307=CARTESIAN_POINT('',(22.3743640879347,-4.5,36.8515390576026));
#7308=CARTESIAN_POINT('Origin',(0.,-6.5,48.6364583401654));
#7309=CARTESIAN_POINT('Origin',(0.,-4.5,48.6364583401654));
#7310=CARTESIAN_POINT('',(17.4118876142729,-6.5,30.2973563844012));
#7311=CARTESIAN_POINT('Origin',(0.,-6.5,48.6364583401654));
#7312=CARTESIAN_POINT('',(17.4118876142729,-2.5,30.2973563844012));
#7313=CARTESIAN_POINT('',(17.4118876142729,-4.5,30.2973563844012));
#7314=CARTESIAN_POINT('Origin',(0.,-2.5,48.6364583401654));
#7315=CARTESIAN_POINT('Origin',(30.9439523809731,-4.5,43.7989769025739));
#7316=CARTESIAN_POINT('',(30.9439523809731,-2.5,43.7989769025739));
#7317=CARTESIAN_POINT('',(15.4016346984504,-2.5,44.400641041252));
#7318=CARTESIAN_POINT('',(30.9439523809731,-6.5,43.7989769025739));
#7319=CARTESIAN_POINT('',(31.2604256489094,-6.5,43.7867257943379));
#7320=CARTESIAN_POINT('',(30.9439523809731,-4.5,43.7989769025739));
#7321=CARTESIAN_POINT('Origin',(30.9558291236816,-4.5,43.697619429073));
#7322=CARTESIAN_POINT('',(30.9558291236816,-2.5,43.697619429073));
#7323=CARTESIAN_POINT('',(30.4607501907366,-2.5,47.9226793683601));
#7324=CARTESIAN_POINT('',(30.9558291236816,-6.5,43.697619429073));
#7325=CARTESIAN_POINT('',(30.8604777930494,-6.5,44.5113585328872));
#7326=CARTESIAN_POINT('',(30.9558291236816,-4.5,43.697619429073));
#7327=CARTESIAN_POINT('Origin',(24.3356530447464,-4.5,41.7609596875797));
#7328=CARTESIAN_POINT('',(24.3356530447464,-2.5,41.7609596875797));
#7329=CARTESIAN_POINT('',(14.0534441823513,-2.5,38.7530125091372));
#7330=CARTESIAN_POINT('',(24.3356530447464,-6.5,41.7609596875797));
#7331=CARTESIAN_POINT('',(31.2604256489094,-6.5,43.7867257943379));
#7332=CARTESIAN_POINT('',(24.3356530447464,-4.5,41.7609596875797));
#7333=CARTESIAN_POINT('Origin',(0.,-4.5,48.6364583401654));
#7334=CARTESIAN_POINT('',(23.3657356055148,-6.5,38.9649077690749));
#7335=CARTESIAN_POINT('Origin',(0.,-6.5,48.6364583401654));
#7336=CARTESIAN_POINT('',(23.3657356055148,-2.5,38.9649077690749));
#7337=CARTESIAN_POINT('',(23.3657356055148,-4.5,38.9649077690749));
#7338=CARTESIAN_POINT('Origin',(0.,-2.5,48.6364583401654));
#7339=CARTESIAN_POINT('Origin',(11.2825943751967,-4.5,19.419468765951));
#7340=CARTESIAN_POINT('',(11.2825943751967,-2.5,19.419468765951));
#7341=CARTESIAN_POINT('',(8.44736607249008,-2.5,24.80080233339));
#7342=CARTESIAN_POINT('',(4.03249196257661,-2.5,33.1803427820428));
#7343=CARTESIAN_POINT('',(8.44736607249008,-6.5,24.80080233339));
#7344=CARTESIAN_POINT('',(8.44736607249008,-4.5,24.80080233339));
#7345=CARTESIAN_POINT('',(11.2825943751967,-6.5,19.419468765951));
#7346=CARTESIAN_POINT('',(11.4302212382079,-6.5,19.1392693221814));
#7347=CARTESIAN_POINT('',(11.2825943751967,-4.5,19.419468765951));
#7348=CARTESIAN_POINT('Origin',(11.2007545996357,-4.5,19.3585044683007));
#7349=CARTESIAN_POINT('',(11.2007545996357,-2.5,19.3585044683007));
#7350=CARTESIAN_POINT('',(14.6122243730978,-2.5,21.8997853707532));
#7351=CARTESIAN_POINT('',(11.2007545996357,-6.5,19.3585044683007));
#7352=CARTESIAN_POINT('',(11.8577976702754,-6.5,19.84795069482));
#7353=CARTESIAN_POINT('',(11.2007545996357,-4.5,19.3585044683007));
#7354=CARTESIAN_POINT('Origin',(6.21347002554836,-4.5,24.123415259438));
#7355=CARTESIAN_POINT('',(6.21347002554835,-2.5,24.123415259438));
#7356=CARTESIAN_POINT('',(-1.53259307542216,-2.5,31.5240957520684));
#7357=CARTESIAN_POINT('',(6.21347002554835,-6.5,24.123415259438));
#7358=CARTESIAN_POINT('',(11.4302212382079,-6.5,19.1392693221814));
#7359=CARTESIAN_POINT('',(6.21347002554835,-4.5,24.123415259438));
#7360=CARTESIAN_POINT('Origin',(0.,-4.5,48.6364583401654));
#7361=CARTESIAN_POINT('',(11.1742390317241,-2.5,25.9509371229247));
#7362=CARTESIAN_POINT('Origin',(0.,-2.5,48.6364583401654));
#7363=CARTESIAN_POINT('',(11.1742390317241,-6.5,25.9509371229247));
#7364=CARTESIAN_POINT('',(11.1742390317241,-4.5,25.9509371229247));
#7365=CARTESIAN_POINT('Origin',(0.,-6.5,48.6364583401654));
#7366=CARTESIAN_POINT('Origin',(0.,-4.5,48.6364583401654));
#7367=CARTESIAN_POINT('',(3.30705931420718,-6.5,23.5653624421338));
#7368=CARTESIAN_POINT('Origin',(0.,-6.5,48.6364583401654));
#7369=CARTESIAN_POINT('',(3.30705931420717,-2.5,23.5653624421338));
#7370=CARTESIAN_POINT('',(3.30705931420717,-4.5,23.5653624421338));
#7371=CARTESIAN_POINT('Origin',(0.,-2.5,48.6364583401654));
#7372=CARTESIAN_POINT('Origin',(29.2619838336808,-4.5,37.4710780182786));
#7373=CARTESIAN_POINT('',(29.2619838336808,-2.5,37.4710780182786));
#7374=CARTESIAN_POINT('',(14.1843960910556,-2.5,41.2910239005742));
#7375=CARTESIAN_POINT('',(29.2619838336808,-6.5,37.4710780182786));
#7376=CARTESIAN_POINT('',(29.5689942527814,-6.5,37.3932961339159));
#7377=CARTESIAN_POINT('',(29.2619838336808,-4.5,37.4710780182786));
#7378=CARTESIAN_POINT('Origin',(29.2525276373731,-4.5,37.3694661350993));
#7379=CARTESIAN_POINT('',(29.2525276373731,-2.5,37.3694661350993));
#7380=CARTESIAN_POINT('',(29.6467067227226,-2.5,41.6051310757064));
#7381=CARTESIAN_POINT('',(29.2525276373731,-6.5,37.3694661350993));
#7382=CARTESIAN_POINT('',(29.3284458350469,-6.5,38.1852477434919));
#7383=CARTESIAN_POINT('',(29.2525276373731,-4.5,37.3694661350993));
#7384=CARTESIAN_POINT('Origin',(22.3743640879348,-4.5,36.8515390576026));
#7385=CARTESIAN_POINT('',(11.6914587751786,-2.5,36.047114171797));
#7386=CARTESIAN_POINT('',(29.5689942527814,-6.5,37.3932961339159));
#7387=CARTESIAN_POINT('Origin',(22.1907831020815,-4.5,26.534454790004));
#7388=CARTESIAN_POINT('',(22.1907831020815,-2.5,26.534454790004));
#7389=CARTESIAN_POINT('',(9.97043327249462,-2.5,36.1567564233319));
#7390=CARTESIAN_POINT('',(22.1907831020815,-6.5,26.534454790004));
#7391=CARTESIAN_POINT('',(22.439614333362,-6.5,26.3385251156033));
#7392=CARTESIAN_POINT('',(22.1907831020815,-4.5,26.534454790004));
#7393=CARTESIAN_POINT('Origin',(22.140815160637,-4.5,26.4454738972255));
#7394=CARTESIAN_POINT('',(22.140815160637,-2.5,26.4454738972255));
#7395=CARTESIAN_POINT('',(24.2237158126922,-2.5,30.1546192858673));
#7396=CARTESIAN_POINT('',(22.140815160637,-6.5,26.4454738972255));
#7397=CARTESIAN_POINT('',(22.541978158155,-6.5,27.1598487671307));
#7398=CARTESIAN_POINT('',(22.140815160637,-4.5,26.4454738972255));
#7399=CARTESIAN_POINT('Origin',(15.6466401722657,-4.5,28.7699251208132));
#7400=CARTESIAN_POINT('',(15.6466401722657,-2.5,28.7699251208132));
#7401=CARTESIAN_POINT('',(5.56013147171207,-2.5,32.3801754655778));
#7402=CARTESIAN_POINT('',(15.6466401722657,-6.5,28.7699251208132));
#7403=CARTESIAN_POINT('',(22.439614333362,-6.5,26.3385251156033));
#7404=CARTESIAN_POINT('',(15.6466401722657,-4.5,28.7699251208132));
#7405=CARTESIAN_POINT('Origin',(0.,-4.5,48.6364583401654));
#7406=CARTESIAN_POINT('',(13.2184823984455,-6.5,27.0779747683097));
#7407=CARTESIAN_POINT('Origin',(0.,-6.5,48.6364583401654));
#7408=CARTESIAN_POINT('',(13.2184823984455,-2.5,27.0779747683097));
#7409=CARTESIAN_POINT('',(13.2184823984455,-4.5,27.0779747683097));
#7410=CARTESIAN_POINT('Origin',(0.,-2.5,48.6364583401654));
#7411=CARTESIAN_POINT('Origin',(30.2362881000144,-4.5,56.8032384613577));
#7412=CARTESIAN_POINT('',(30.2362881000144,-2.5,56.8032384613577));
#7413=CARTESIAN_POINT('',(24.5880719834211,-2.5,54.5460443640832));
#7414=CARTESIAN_POINT('',(15.7929555278825,-2.5,51.0312558824666));
#7415=CARTESIAN_POINT('',(24.5880719834211,-6.5,54.5460443640832));
#7416=CARTESIAN_POINT('',(24.5880719834211,-4.5,54.5460443640832));
#7417=CARTESIAN_POINT('',(30.2362881000144,-6.5,56.8032384613577));
#7418=CARTESIAN_POINT('',(30.5303837910408,-6.5,56.9207677917012));
#7419=CARTESIAN_POINT('',(30.2362881000144,-4.5,56.8032384613577));
#7420=CARTESIAN_POINT('Origin',(30.2883638428897,-4.5,56.7154745083027));
#7421=CARTESIAN_POINT('',(30.2883638428897,-2.5,56.7154745083027));
#7422=CARTESIAN_POINT('',(28.1176000360236,-2.5,60.3738920808626));
#7423=CARTESIAN_POINT('',(30.2883638428897,-6.5,56.7154745083027));
#7424=CARTESIAN_POINT('',(29.8702785564856,-6.5,57.4200792901642));
#7425=CARTESIAN_POINT('',(30.2883638428897,-4.5,56.7154745083027));
#7426=CARTESIAN_POINT('Origin',(25.0282425392193,-4.5,52.2535796035455));
#7427=CARTESIAN_POINT('',(16.8584196763548,-2.5,45.3235320057556));
#7428=CARTESIAN_POINT('',(30.5303837910408,-6.5,56.9207677917012));
#7429=CARTESIAN_POINT('Origin',(0.,-4.5,48.6364583401654));
#7430=CARTESIAN_POINT('',(23.7292735925589,-2.5,57.3782010500299));
#7431=CARTESIAN_POINT('Origin',(0.,-2.5,48.6364583401654));
#7432=CARTESIAN_POINT('',(23.7292735925589,-6.5,57.3782010500299));
#7433=CARTESIAN_POINT('',(23.7292735925589,-4.5,57.3782010500299));
#7434=CARTESIAN_POINT('Origin',(0.,-6.5,48.6364583401654));
#7435=CARTESIAN_POINT('Origin',(17.1105963211311,-4.5,22.403713360841));
#7436=CARTESIAN_POINT('',(17.1105963211311,-2.5,22.403713360841));
#7437=CARTESIAN_POINT('',(7.15787945733662,-2.5,34.3564982124716));
#7438=CARTESIAN_POINT('',(17.1105963211311,-6.5,22.403713360841));
#7439=CARTESIAN_POINT('',(17.3132539231097,-6.5,22.1603302978897));
#7440=CARTESIAN_POINT('',(17.1105963211311,-4.5,22.403713360841));
#7441=CARTESIAN_POINT('Origin',(17.0432201312255,-4.5,22.327065833251));
#7442=CARTESIAN_POINT('',(17.0432201312255,-2.5,22.327065833251));
#7443=CARTESIAN_POINT('',(19.8517790958416,-2.5,25.5220980995497));
#7444=CARTESIAN_POINT('',(17.0432201312255,-6.5,22.327065833251));
#7445=CARTESIAN_POINT('',(17.5841436418306,-6.5,22.9424234211658));
#7446=CARTESIAN_POINT('',(17.0432201312255,-4.5,22.327065833251));
#7447=CARTESIAN_POINT('Origin',(11.1742390317241,-4.5,25.9509371229247));
#7448=CARTESIAN_POINT('',(2.05875799995238,-2.5,31.5793979140848));
#7449=CARTESIAN_POINT('',(17.3132539231097,-6.5,22.1603302978897));
#7450=CARTESIAN_POINT('Origin',(4.57790069807404,-4.5,42.4313271208406));
#7451=CARTESIAN_POINT('',(13.6784299900821,-2.5,32.3241653975668));
#7452=CARTESIAN_POINT('',(4.57790069807404,-2.5,42.4313271208406));
#7453=CARTESIAN_POINT('',(2.010271039483,-2.5,45.2829687531184));
#7454=CARTESIAN_POINT('',(13.6784299900821,-6.5,32.3241653975668));
#7455=CARTESIAN_POINT('',(13.6784299900821,-4.5,32.3241653975668));
#7456=CARTESIAN_POINT('',(4.57790069807404,-6.5,42.4313271208406));
#7457=CARTESIAN_POINT('',(13.6784299900821,-6.5,32.3241653975668));
#7458=CARTESIAN_POINT('',(4.57790069807404,-4.5,42.4313271208406));
#7459=CARTESIAN_POINT('Origin',(14.7931472282982,-4.5,33.3278613071051));
#7460=CARTESIAN_POINT('',(5.69261793629013,-2.5,43.4350230303789));
#7461=CARTESIAN_POINT('',(14.7931472282982,-2.5,33.3278613071051));
#7462=CARTESIAN_POINT('',(7.67525292370313,-2.5,41.2330838010198));
#7463=CARTESIAN_POINT('',(5.69261793629014,-6.5,43.4350230303789));
#7464=CARTESIAN_POINT('',(5.69261793629013,-4.5,43.4350230303789));
#7465=CARTESIAN_POINT('',(14.7931472282982,-6.5,33.3278613071051));
#7466=CARTESIAN_POINT('',(5.69261793629014,-6.5,43.4350230303789));
#7467=CARTESIAN_POINT('',(14.7931472282982,-4.5,33.3278613071051));
#7468=CARTESIAN_POINT('Origin',(0.,-4.5,48.6364583401654));
#7469=CARTESIAN_POINT('',(7.28764508722295,-2.5,28.6344440135681));
#7470=CARTESIAN_POINT('Origin',(0.,-2.5,48.6364583401654));
#7471=CARTESIAN_POINT('',(7.28764508722295,-6.5,28.6344440135681));
#7472=CARTESIAN_POINT('',(7.28764508722295,-4.5,28.6344440135681));
#7473=CARTESIAN_POINT('Origin',(0.,-6.5,48.6364583401654));
#7474=CARTESIAN_POINT('Origin',(0.,-4.5,48.6364583401654));
#7475=CARTESIAN_POINT('',(19.1306748574635,-6.5,39.2979559154323));
#7476=CARTESIAN_POINT('Origin',(0.,-6.5,48.6364583401654));
#7477=CARTESIAN_POINT('',(19.1306748574635,-2.5,39.2979559154323));
#7478=CARTESIAN_POINT('',(19.1306748574635,-4.5,39.2979559154323));
#7479=CARTESIAN_POINT('Origin',(0.,-2.5,48.6364583401654));
#7480=CARTESIAN_POINT('Origin',(0.,-4.5,48.6364583401654));
#7481=CARTESIAN_POINT('',(3.08485092071416,-6.5,41.5693144299684));
#7482=CARTESIAN_POINT('Origin',(0.,-6.5,48.6364583401654));
#7483=CARTESIAN_POINT('',(3.08485092071416,-2.5,41.5693144299684));
#7484=CARTESIAN_POINT('',(3.08485092071416,-4.5,41.5693144299684));
#7485=CARTESIAN_POINT('Origin',(0.,-2.5,48.6364583401654));
#7486=CARTESIAN_POINT('Origin',(0.,-4.5,48.6364583401654));
#7487=CARTESIAN_POINT('',(6.70597463025744,-2.5,44.8297888629439));
#7488=CARTESIAN_POINT('Origin',(0.,-2.5,48.6364583401654));
#7489=CARTESIAN_POINT('',(6.70597463025745,-6.5,44.8297888629439));
#7490=CARTESIAN_POINT('',(6.70597463025744,-4.5,44.8297888629439));
#7491=CARTESIAN_POINT('Origin',(0.,-6.5,48.6364583401654));
#7492=CARTESIAN_POINT('Origin',(6.70597463025745,-4.5,44.8297888629439));
#7493=CARTESIAN_POINT('',(3.2004610739753,-2.5,46.3905440549387));
#7494=CARTESIAN_POINT('',(19.1306748574635,-6.5,39.2979559154323));
#7495=CARTESIAN_POINT('Origin',(19.7407798220772,-4.5,40.6682741018962));
#7496=CARTESIAN_POINT('',(7.31607959487115,-2.5,46.2001070494078));
#7497=CARTESIAN_POINT('',(19.7407798220772,-2.5,40.6682741018962));
#7498=CARTESIAN_POINT('',(10.022916152192,-2.5,44.9949457676468));
#7499=CARTESIAN_POINT('',(7.31607959487115,-6.5,46.2001070494078));
#7500=CARTESIAN_POINT('',(7.31607959487115,-4.5,46.2001070494078));
#7501=CARTESIAN_POINT('',(19.7407798220772,-6.5,40.6682741018962));
#7502=CARTESIAN_POINT('',(7.31607959487115,-6.5,46.2001070494078));
#7503=CARTESIAN_POINT('',(19.7407798220772,-4.5,40.6682741018962));
#7504=CARTESIAN_POINT('Origin',(0.,-4.5,48.6364583401654));
#7505=CARTESIAN_POINT('',(21.2750522452644,-6.5,47.8864583401654));
#7506=CARTESIAN_POINT('Origin',(0.,-6.5,48.6364583401654));
#7507=CARTESIAN_POINT('',(21.2750522452644,-2.5,47.8864583401654));
#7508=CARTESIAN_POINT('',(21.2750522452644,-4.5,47.8864583401654));
#7509=CARTESIAN_POINT('Origin',(0.,-2.5,48.6364583401654));
#7510=CARTESIAN_POINT('Origin',(0.,-4.5,48.6364583401654));
#7511=CARTESIAN_POINT('',(7.67452462700238,-2.5,47.8864583401654));
#7512=CARTESIAN_POINT('Origin',(0.,-2.5,48.6364583401654));
#7513=CARTESIAN_POINT('',(7.67452462700238,-6.5,47.8864583401654));
#7514=CARTESIAN_POINT('',(7.67452462700238,-4.5,47.8864583401654));
#7515=CARTESIAN_POINT('Origin',(0.,-6.5,48.6364583401654));
#7516=CARTESIAN_POINT('Origin',(1.65826614627142,-4.5,41.1057889384059));
#7517=CARTESIAN_POINT('',(5.86106031278022,-2.5,28.1709185220056));
#7518=CARTESIAN_POINT('',(1.65826614627142,-2.5,41.1057889384059));
#7519=CARTESIAN_POINT('',(0.472486879525025,-2.5,44.7552422663951));
#7520=CARTESIAN_POINT('',(5.86106031278022,-6.5,28.1709185220056));
#7521=CARTESIAN_POINT('',(5.86106031278022,-4.5,28.1709185220056));
#7522=CARTESIAN_POINT('',(1.65826614627142,-6.5,41.1057889384059));
#7523=CARTESIAN_POINT('',(5.86106031278022,-6.5,28.1709185220056));
#7524=CARTESIAN_POINT('',(1.65826614627142,-4.5,41.1057889384059));
#7525=CARTESIAN_POINT('Origin',(7.28764508722295,-4.5,28.6344440135681));
#7526=CARTESIAN_POINT('',(4.00046873722216,-2.5,38.7513325497573));
#7527=CARTESIAN_POINT('',(3.08485092071416,-6.5,41.5693144299684));
#7528=CARTESIAN_POINT('Origin',(0.,-4.5,48.6364583401654));
#7529=CARTESIAN_POINT('',(-1.47795709561032,-2.5,27.3995567096953));
#7530=CARTESIAN_POINT('Origin',(0.,-2.5,48.6364583401654));
#7531=CARTESIAN_POINT('',(-1.47795709561032,-6.5,27.3995567096953));
#7532=CARTESIAN_POINT('',(-1.47795709561032,-4.5,27.3995567096953));
#7533=CARTESIAN_POINT('Origin',(0.,-6.5,48.6364583401654));
#7534=CARTESIAN_POINT('Origin',(0.,-4.5,48.6364583401654));
#7535=CARTESIAN_POINT('',(-0.0563148440441186,-6.5,40.9255792146178));
#7536=CARTESIAN_POINT('Origin',(0.,-6.5,48.6364583401654));
#7537=CARTESIAN_POINT('',(-0.0563148440441168,-2.5,40.9255792146178));
#7538=CARTESIAN_POINT('',(-0.0563148440441168,-4.5,40.9255792146178));
#7539=CARTESIAN_POINT('Origin',(0.,-2.5,48.6364583401654));
#7540=CARTESIAN_POINT('Origin',(19.6613580057765,-4.5,73.0159664767883));
#7541=CARTESIAN_POINT('',(19.6613580057765,-2.5,73.0159664767883));
#7542=CARTESIAN_POINT('',(16.4186005814896,-2.5,67.8699199573963));
#7543=CARTESIAN_POINT('',(11.3691427358738,-2.5,59.8567565993746));
#7544=CARTESIAN_POINT('',(16.4186005814896,-6.5,67.8699199573963));
#7545=CARTESIAN_POINT('',(16.4186005814896,-4.5,67.8699199573963));
#7546=CARTESIAN_POINT('',(19.6613580057765,-6.5,73.0159664767883));
#7547=CARTESIAN_POINT('',(19.8302044107015,-6.5,73.2839148123218));
#7548=CARTESIAN_POINT('',(19.6613580057765,-4.5,73.0159664767883));
#7549=CARTESIAN_POINT('Origin',(19.7550745240459,-4.5,72.9755733009377));
#7550=CARTESIAN_POINT('',(19.7550745240459,-2.5,72.9755733009377));
#7551=CARTESIAN_POINT('',(15.8485258176388,-2.5,74.6593523377723));
#7552=CARTESIAN_POINT('',(19.7550745240459,-6.5,72.9755733009377));
#7553=CARTESIAN_POINT('',(19.0026801227739,-6.5,73.2998661782326));
#7554=CARTESIAN_POINT('',(19.7550745240459,-4.5,72.9755733009377));
#7555=CARTESIAN_POINT('Origin',(18.1221830191981,-4.5,66.2740027683071));
#7556=CARTESIAN_POINT('',(18.1221830191981,-2.5,66.2740027683071));
#7557=CARTESIAN_POINT('',(15.5860372577735,-2.5,55.8653750972342));
#7558=CARTESIAN_POINT('',(18.1221830191981,-6.5,66.2740027683071));
#7559=CARTESIAN_POINT('',(19.8302044107015,-6.5,73.2839148123218));
#7560=CARTESIAN_POINT('',(18.1221830191981,-4.5,66.2740027683071));
#7561=CARTESIAN_POINT('Origin',(0.,-4.5,48.6364583401654));
#7562=CARTESIAN_POINT('',(14.0591181563592,-2.5,69.6563938182185));
#7563=CARTESIAN_POINT('Origin',(0.,-2.5,48.6364583401654));
#7564=CARTESIAN_POINT('',(14.0591181563592,-6.5,69.6563938182185));
#7565=CARTESIAN_POINT('',(14.0591181563592,-4.5,69.6563938182185));
#7566=CARTESIAN_POINT('Origin',(0.,-6.5,48.6364583401654));
#7567=CARTESIAN_POINT('Origin',(0.,-4.5,48.6364583401654));
#7568=CARTESIAN_POINT('',(20.0586762913077,-6.5,64.0360036671066));
#7569=CARTESIAN_POINT('Origin',(0.,-6.5,48.6364583401654));
#7570=CARTESIAN_POINT('',(20.0586762913077,-2.5,64.0360036671066));
#7571=CARTESIAN_POINT('',(20.0586762913077,-4.5,64.0360036671066));
#7572=CARTESIAN_POINT('Origin',(0.,-2.5,48.6364583401654));
#7573=CARTESIAN_POINT('Origin',(1.57645741831176,-4.5,79.9165510130336));
#7574=CARTESIAN_POINT('',(1.57645741831176,-2.5,79.9165510130336));
#7575=CARTESIAN_POINT('',(1.97778180513783,-2.5,73.8472669342436));
#7576=CARTESIAN_POINT('',(2.60270384171029,-2.5,64.396484745176));
#7577=CARTESIAN_POINT('',(1.97778180513783,-6.5,73.8472669342436));
#7578=CARTESIAN_POINT('',(1.97778180513783,-4.5,73.8472669342436));
#7579=CARTESIAN_POINT('',(1.57645741831176,-6.5,79.9165510130336));
#7580=CARTESIAN_POINT('',(1.55556094933236,-6.5,80.2325711968123));
#7581=CARTESIAN_POINT('',(1.57645741831176,-4.5,79.9165510130336));
#7582=CARTESIAN_POINT('Origin',(1.67601818730369,-4.5,79.9389574346486));
#7583=CARTESIAN_POINT('',(1.67601818730369,-2.5,79.9389574346486));
#7584=CARTESIAN_POINT('',(-2.47414659150375,-2.5,79.0049515732318));
#7585=CARTESIAN_POINT('',(1.67601818730369,-6.5,79.9389574346486));
#7586=CARTESIAN_POINT('',(0.876703759504667,-6.5,79.7590695505599));
#7587=CARTESIAN_POINT('',(1.67601818730369,-4.5,79.9389574346486));
#7588=CARTESIAN_POINT('Origin',(4.29406553618938,-4.5,73.5574834396049));
#7589=CARTESIAN_POINT('',(4.29406553618938,-2.5,73.5574834396049));
#7590=CARTESIAN_POINT('',(8.3603183566449,-2.5,63.6460176893561));
#7591=CARTESIAN_POINT('',(4.29406553618938,-6.5,73.5574834396049));
#7592=CARTESIAN_POINT('',(1.55556094933236,-6.5,80.2325711968123));
#7593=CARTESIAN_POINT('',(4.29406553618938,-4.5,73.5574834396049));
#7594=CARTESIAN_POINT('Origin',(0.,-4.5,48.6364583401654));
#7595=CARTESIAN_POINT('',(-0.981142563718944,-2.5,73.9056856751205));
#7596=CARTESIAN_POINT('Origin',(0.,-2.5,48.6364583401654));
#7597=CARTESIAN_POINT('',(-0.981142563718944,-6.5,73.9056856751205));
#7598=CARTESIAN_POINT('',(-0.981142563718944,-4.5,73.9056856751205));
#7599=CARTESIAN_POINT('Origin',(0.,-6.5,48.6364583401654));
#7600=CARTESIAN_POINT('Origin',(0.,-4.5,48.6364583401654));
#7601=CARTESIAN_POINT('',(7.17618436914825,-6.5,72.8851463198474));
#7602=CARTESIAN_POINT('Origin',(0.,-6.5,48.6364583401654));
#7603=CARTESIAN_POINT('',(7.17618436914825,-2.5,72.8851463198474));
#7604=CARTESIAN_POINT('',(7.17618436914825,-4.5,72.8851463198474));
#7605=CARTESIAN_POINT('Origin',(0.,-2.5,48.6364583401654));
#7606=CARTESIAN_POINT('Origin',(8.04550499793291,-4.5,78.9052420115192));
#7607=CARTESIAN_POINT('',(8.04550499793291,-2.5,78.9052420115191));
#7608=CARTESIAN_POINT('',(5.82252225538788,-2.5,63.5109577993001));
#7609=CARTESIAN_POINT('',(8.04550499793291,-6.5,78.9052420115191));
#7610=CARTESIAN_POINT('',(8.09076945767885,-6.5,79.2187010162633));
#7611=CARTESIAN_POINT('',(8.04550499793291,-4.5,78.9052420115191));
#7612=CARTESIAN_POINT('Origin',(8.14754868225272,-4.5,78.9064589512426));
#7613=CARTESIAN_POINT('',(8.14754868225272,-2.5,78.9064589512426));
#7614=CARTESIAN_POINT('',(3.89388422333141,-2.5,78.8557311351607));
#7615=CARTESIAN_POINT('',(8.14754868225272,-6.5,78.9064589512426));
#7616=CARTESIAN_POINT('',(7.32830039833067,-6.5,78.8966888631989));
#7617=CARTESIAN_POINT('',(8.14754868225272,-4.5,78.9064589512426));
#7618=CARTESIAN_POINT('Origin',(9.38160236695365,-4.5,72.1201128228977));
#7619=CARTESIAN_POINT('',(9.38160236695366,-2.5,72.1201128228977));
#7620=CARTESIAN_POINT('',(11.2982882046428,-2.5,61.5798148803432));
#7621=CARTESIAN_POINT('',(9.38160236695365,-6.5,72.1201128228977));
#7622=CARTESIAN_POINT('',(8.09076945767885,-6.5,79.2187010162633));
#7623=CARTESIAN_POINT('',(9.38160236695366,-4.5,72.1201128228977));
#7624=CARTESIAN_POINT('Origin',(0.,-4.5,48.6364583401654));
#7625=CARTESIAN_POINT('',(12.0609532410738,-6.5,70.8632416826245));
#7626=CARTESIAN_POINT('Origin',(0.,-6.5,48.6364583401654));
#7627=CARTESIAN_POINT('',(12.0609532410738,-2.5,70.8632416826245));
#7628=CARTESIAN_POINT('',(12.0609532410738,-4.5,70.8632416826245));
#7629=CARTESIAN_POINT('Origin',(0.,-2.5,48.6364583401654));
#7630=CARTESIAN_POINT('Origin',(14.162925402528,-4.5,76.5710419178277));
#7631=CARTESIAN_POINT('',(14.162925402528,-2.5,76.5710419178277));
#7632=CARTESIAN_POINT('',(8.78786850694337,-2.5,61.9753438512926));
#7633=CARTESIAN_POINT('',(14.162925402528,-6.5,76.5710419178277));
#7634=CARTESIAN_POINT('',(14.2723725169055,-6.5,76.8682400808869));
#7635=CARTESIAN_POINT('',(14.162925402528,-4.5,76.5710419178277));
#7636=CARTESIAN_POINT('Origin',(14.262992203511,-4.5,76.5510161895543));
#7637=CARTESIAN_POINT('',(14.262992203511,-2.5,76.5510161895543));
#7638=CARTESIAN_POINT('',(10.0917336126774,-2.5,77.385783467789));
#7639=CARTESIAN_POINT('',(14.262992203511,-6.5,76.5510161895543));
#7640=CARTESIAN_POINT('',(13.4596151446628,-6.5,76.7117908972851));
#7641=CARTESIAN_POINT('',(14.262992203511,-4.5,76.5510161895543));
#7642=CARTESIAN_POINT('Origin',(14.0591181563592,-4.5,69.6563938182185));
#7643=CARTESIAN_POINT('',(13.7424686428958,-2.5,58.9479252814089));
#7644=CARTESIAN_POINT('',(14.2723725169055,-6.5,76.8682400808869));
#7645=CARTESIAN_POINT('Origin',(24.3004949185093,-4.5,68.3953895443191));
#7646=CARTESIAN_POINT('',(24.3004949185093,-2.5,68.3953895443191));
#7647=CARTESIAN_POINT('',(13.4535308720469,-2.5,57.2477884725646));
#7648=CARTESIAN_POINT('',(24.3004949185093,-6.5,68.3953895443191));
#7649=CARTESIAN_POINT('',(24.5213612158718,-6.5,68.6223774243054));
#7650=CARTESIAN_POINT('',(24.3004949185093,-4.5,68.3953895443191));
#7651=CARTESIAN_POINT('Origin',(24.383765292515,-4.5,68.3363942965038));
#7652=CARTESIAN_POINT('',(24.383765292515,-2.5,68.3363942965038));
#7653=CARTESIAN_POINT('',(20.912661394705,-2.5,70.7955958683606));
#7654=CARTESIAN_POINT('',(24.383765292515,-6.5,68.3363942965038));
#7655=CARTESIAN_POINT('',(23.7152367945438,-6.5,68.8100321884952));
#7656=CARTESIAN_POINT('',(24.383765292515,-4.5,68.3363942965038));
#7657=CARTESIAN_POINT('Origin',(21.3932215242158,-4.5,62.1207663925577));
#7658=CARTESIAN_POINT('',(21.3932215242158,-2.5,62.1207663925577));
#7659=CARTESIAN_POINT('',(16.7484212543818,-2.5,52.4668865625843));
#7660=CARTESIAN_POINT('',(21.3932215242158,-6.5,62.1207663925577));
#7661=CARTESIAN_POINT('',(24.5213612158718,-6.5,68.6223774243054));
#7662=CARTESIAN_POINT('',(21.3932215242158,-4.5,62.1207663925577));
#7663=CARTESIAN_POINT('Origin',(0.,-4.5,48.6364583401654));
#7664=CARTESIAN_POINT('',(22.8220915949877,-6.5,59.5290533508125));
#7665=CARTESIAN_POINT('Origin',(0.,-6.5,48.6364583401654));
#7666=CARTESIAN_POINT('',(22.8220915949877,-2.5,59.5290533508125));
#7667=CARTESIAN_POINT('',(22.8220915949877,-4.5,59.5290533508125));
#7668=CARTESIAN_POINT('Origin',(0.,-2.5,48.6364583401654));
#7669=CARTESIAN_POINT('Origin',(27.8775835965913,-4.5,62.9112525043571));
#7670=CARTESIAN_POINT('',(27.8775835965913,-2.5,62.9112525043571));
#7671=CARTESIAN_POINT('',(14.9499351519079,-2.5,54.2624638972222));
#7672=CARTESIAN_POINT('',(27.8775835965913,-6.5,62.9112525043571));
#7673=CARTESIAN_POINT('',(28.1408168693625,-6.5,63.087359469232));
#7674=CARTESIAN_POINT('',(27.8775835965913,-4.5,62.9112525043571));
#7675=CARTESIAN_POINT('Origin',(27.9467685114137,-4.5,62.8362335599973));
#7676=CARTESIAN_POINT('',(27.9467685114137,-2.5,62.8362335599973));
#7677=CARTESIAN_POINT('',(25.0628133187395,-2.5,65.9633787576275));
#7678=CARTESIAN_POINT('',(27.9467685114137,-6.5,62.8362335599973));
#7679=CARTESIAN_POINT('',(27.3913238200603,-6.5,63.4385162180383));
#7680=CARTESIAN_POINT('',(27.9467685114137,-4.5,62.8362335599973));
#7681=CARTESIAN_POINT('Origin',(23.7292735925589,-4.5,57.3782010500299));
#7682=CARTESIAN_POINT('',(17.1788188743319,-2.5,48.9009899341809));
#7683=CARTESIAN_POINT('',(28.1408168693625,-6.5,63.087359469232));
#7684=CARTESIAN_POINT('Origin',(-3.18774326066286,-4.5,55.6577916291187));
#7685=CARTESIAN_POINT('',(-9.98800706979388,-2.5,67.4361940514055));
#7686=CARTESIAN_POINT('',(-3.18774326066286,-2.5,55.6577916291187));
#7687=CARTESIAN_POINT('',(-1.26911210391227,-2.5,52.3346249846421));
#7688=CARTESIAN_POINT('',(-9.98800706979389,-6.5,67.4361940514055));
#7689=CARTESIAN_POINT('',(-9.98800706979388,-4.5,67.4361940514055));
#7690=CARTESIAN_POINT('',(-3.18774326066286,-6.5,55.6577916291187));
#7691=CARTESIAN_POINT('',(-9.98800706979389,-6.5,67.4361940514055));
#7692=CARTESIAN_POINT('',(-3.18774326066286,-4.5,55.6577916291187));
#7693=CARTESIAN_POINT('Origin',(-11.2870451754705,-4.5,66.6861940514055));
#7694=CARTESIAN_POINT('',(-4.48678136633952,-2.5,54.9077916291187));
#7695=CARTESIAN_POINT('',(-11.2870451754705,-2.5,66.6861940514055));
#7696=CARTESIAN_POINT('',(-5.96828211415444,-2.5,57.4738261957855));
#7697=CARTESIAN_POINT('',(-4.48678136633952,-6.5,54.9077916291187));
#7698=CARTESIAN_POINT('',(-4.48678136633952,-4.5,54.9077916291187));
#7699=CARTESIAN_POINT('',(-11.2870451754705,-6.5,66.6861940514055));
#7700=CARTESIAN_POINT('',(-4.48678136633952,-6.5,54.9077916291187));
#7701=CARTESIAN_POINT('',(-11.2870451754705,-4.5,66.6861940514055));
#7702=CARTESIAN_POINT('Origin',(0.,-4.5,48.6364583401654));
#7703=CARTESIAN_POINT('',(-2.96973993866275,-2.5,69.7165672757341));
#7704=CARTESIAN_POINT('Origin',(0.,-2.5,48.6364583401654));
#7705=CARTESIAN_POINT('',(-2.96973993866275,-6.5,69.7165672757341));
#7706=CARTESIAN_POINT('',(-2.96973993866275,-4.5,69.7165672757341));
#7707=CARTESIAN_POINT('Origin',(0.,-6.5,48.6364583401654));
#7708=CARTESIAN_POINT('Origin',(0.,-4.5,48.6364583401654));
#7709=CARTESIAN_POINT('',(-16.7710398834144,-6.5,61.7483830374649));
#7710=CARTESIAN_POINT('Origin',(0.,-6.5,48.6364583401654));
#7711=CARTESIAN_POINT('',(-16.7710398834144,-2.5,61.7483830374649));
#7712=CARTESIAN_POINT('',(-16.7710398834144,-4.5,61.7483830374649));
#7713=CARTESIAN_POINT('Origin',(0.,-2.5,48.6364583401654));
#7714=CARTESIAN_POINT('Origin',(0.,-4.5,48.6364583401654));
#7715=CARTESIAN_POINT('',(-1.54809768709653,-6.5,56.1905447708115));
#7716=CARTESIAN_POINT('Origin',(0.,-6.5,48.6364583401654));
#7717=CARTESIAN_POINT('',(-1.54809768709653,-2.5,56.1905447708115));
#7718=CARTESIAN_POINT('',(-1.54809768709653,-4.5,56.1905447708115));
#7719=CARTESIAN_POINT('Origin',(0.,-2.5,48.6364583401654));
#7720=CARTESIAN_POINT('Origin',(0.,-4.5,48.6364583401654));
#7721=CARTESIAN_POINT('',(-5.76798190777462,-2.5,53.754193480054));
#7722=CARTESIAN_POINT('Origin',(0.,-2.5,48.6364583401654));
#7723=CARTESIAN_POINT('',(-5.76798190777462,-6.5,53.754193480054));
#7724=CARTESIAN_POINT('',(-5.76798190777462,-4.5,53.754193480054));
#7725=CARTESIAN_POINT('Origin',(0.,-6.5,48.6364583401654));
#7726=CARTESIAN_POINT('Origin',(-5.76798190777462,-4.5,53.754193480054));
#7727=CARTESIAN_POINT('',(-2.66357148427763,-2.5,51.4987072830003));
#7728=CARTESIAN_POINT('',(-16.7710398834144,-6.5,61.7483830374649));
#7729=CARTESIAN_POINT('Origin',(-17.6527177618532,-4.5,60.5348575459025));
#7730=CARTESIAN_POINT('',(-6.64965978621333,-2.5,52.5406679884916));
#7731=CARTESIAN_POINT('',(-17.6527177618531,-2.5,60.5348575459025));
#7732=CARTESIAN_POINT('',(-9.04677835053625,-2.5,54.2822765701433));
#7733=CARTESIAN_POINT('',(-6.64965978621333,-6.5,52.5406679884916));
#7734=CARTESIAN_POINT('',(-6.64965978621333,-4.5,52.5406679884916));
#7735=CARTESIAN_POINT('',(-17.6527177618532,-6.5,60.5348575459025));
#7736=CARTESIAN_POINT('',(-6.64965978621333,-6.5,52.5406679884916));
#7737=CARTESIAN_POINT('',(-17.6527177618531,-4.5,60.5348575459025));
#7738=CARTESIAN_POINT('Origin',(0.,-4.5,48.6364583401654));
#7739=CARTESIAN_POINT('',(-20.6542075410784,-6.5,53.7934011252648));
#7740=CARTESIAN_POINT('Origin',(0.,-6.5,48.6364583401654));
#7741=CARTESIAN_POINT('',(-20.6542075410784,-2.5,53.7934011252648));
#7742=CARTESIAN_POINT('',(-20.6542075410784,-4.5,53.7934011252648));
#7743=CARTESIAN_POINT('Origin',(0.,-2.5,48.6364583401654));
#7744=CARTESIAN_POINT('Origin',(0.,-4.5,48.6364583401654));
#7745=CARTESIAN_POINT('',(-7.35088408256156,-2.5,50.9656924321383));
#7746=CARTESIAN_POINT('Origin',(0.,-2.5,48.6364583401654));
#7747=CARTESIAN_POINT('',(-7.35088408256156,-6.5,50.9656924321383));
#7748=CARTESIAN_POINT('',(-7.35088408256156,-4.5,50.9656924321383));
#7749=CARTESIAN_POINT('Origin',(0.,-6.5,48.6364583401654));
#7750=CARTESIAN_POINT('Origin',(3.08485092071416,-4.5,55.7036022503624));
#7751=CARTESIAN_POINT('',(7.28764508722295,-2.5,68.6384726667627));
#7752=CARTESIAN_POINT('',(3.08485092071415,-2.5,55.7036022503624));
#7753=CARTESIAN_POINT('',(1.89907165396776,-2.5,52.0541489223733));
#7754=CARTESIAN_POINT('',(7.28764508722294,-6.5,68.6384726667627));
#7755=CARTESIAN_POINT('',(7.28764508722295,-4.5,68.6384726667627));
#7756=CARTESIAN_POINT('',(3.08485092071416,-6.5,55.7036022503624));
#7757=CARTESIAN_POINT('',(7.28764508722294,-6.5,68.6384726667627));
#7758=CARTESIAN_POINT('',(3.08485092071415,-4.5,55.7036022503624));
#7759=CARTESIAN_POINT('Origin',(5.86106031278021,-4.5,69.1019981583252));
#7760=CARTESIAN_POINT('',(1.65826614627142,-2.5,56.1671277419249));
#7761=CARTESIAN_POINT('',(5.86106031278021,-2.5,69.1019981583252));
#7762=CARTESIAN_POINT('',(2.57388396277942,-2.5,58.9851096221359));
#7763=CARTESIAN_POINT('',(1.65826614627142,-6.5,56.1671277419249));
#7764=CARTESIAN_POINT('',(1.65826614627142,-4.5,56.1671277419249));
#7765=CARTESIAN_POINT('',(5.86106031278021,-6.5,69.1019981583252));
#7766=CARTESIAN_POINT('',(1.65826614627142,-6.5,56.1671277419249));
#7767=CARTESIAN_POINT('',(5.86106031278021,-4.5,69.1019981583252));
#7768=CARTESIAN_POINT('Origin',(0.,-4.5,48.6364583401654));
#7769=CARTESIAN_POINT('',(13.6784299900821,-2.5,64.948751282764));
#7770=CARTESIAN_POINT('Origin',(0.,-2.5,48.6364583401654));
#7771=CARTESIAN_POINT('',(13.6784299900821,-6.5,64.948751282764));
#7772=CARTESIAN_POINT('',(13.6784299900821,-4.5,64.948751282764));
#7773=CARTESIAN_POINT('Origin',(0.,-6.5,48.6364583401654));
#7774=CARTESIAN_POINT('Origin',(0.,-4.5,48.6364583401654));
#7775=CARTESIAN_POINT('',(-1.47795709561033,-6.5,69.8733599706355));
#7776=CARTESIAN_POINT('Origin',(0.,-6.5,48.6364583401654));
#7777=CARTESIAN_POINT('',(-1.47795709561034,-2.5,69.8733599706355));
#7778=CARTESIAN_POINT('',(-1.47795709561034,-4.5,69.8733599706355));
#7779=CARTESIAN_POINT('Origin',(0.,-2.5,48.6364583401654));
#7780=CARTESIAN_POINT('Origin',(0.,-4.5,48.6364583401654));
#7781=CARTESIAN_POINT('',(4.57790069807404,-6.5,54.8415895594902));
#7782=CARTESIAN_POINT('Origin',(0.,-6.5,48.6364583401654));
#7783=CARTESIAN_POINT('',(4.57790069807404,-2.5,54.8415895594902));
#7784=CARTESIAN_POINT('',(4.57790069807404,-4.5,54.8415895594902));
#7785=CARTESIAN_POINT('Origin',(0.,-2.5,48.6364583401654));
#7786=CARTESIAN_POINT('Origin',(0.,-4.5,48.6364583401654));
#7787=CARTESIAN_POINT('',(-0.0563148440441184,-2.5,56.347337465713));
#7788=CARTESIAN_POINT('Origin',(0.,-2.5,48.6364583401654));
#7789=CARTESIAN_POINT('',(-0.0563148440441186,-6.5,56.347337465713));
#7790=CARTESIAN_POINT('',(-0.0563148440441184,-4.5,56.347337465713));
#7791=CARTESIAN_POINT('Origin',(0.,-6.5,48.6364583401654));
#7792=CARTESIAN_POINT('Origin',(7.31607959487115,-4.5,51.0728096309229));
#7793=CARTESIAN_POINT('',(19.7407798220772,-2.5,56.6046425784346));
#7794=CARTESIAN_POINT('',(7.31607959487115,-2.5,51.0728096309229));
#7795=CARTESIAN_POINT('',(3.810566038589,-2.5,49.5120544389282));
#7796=CARTESIAN_POINT('',(19.7407798220772,-6.5,56.6046425784346));
#7797=CARTESIAN_POINT('',(19.7407798220772,-4.5,56.6046425784346));
#7798=CARTESIAN_POINT('',(7.31607959487115,-6.5,51.0728096309229));
#7799=CARTESIAN_POINT('',(19.7407798220772,-6.5,56.6046425784346));
#7800=CARTESIAN_POINT('',(7.31607959487115,-4.5,51.0728096309229));
#7801=CARTESIAN_POINT('Origin',(19.1306748574635,-4.5,57.9749607648985));
#7802=CARTESIAN_POINT('',(6.70597463025744,-2.5,52.4431278173869));
#7803=CARTESIAN_POINT('',(19.1306748574635,-2.5,57.9749607648985));
#7804=CARTESIAN_POINT('',(9.41281118757831,-2.5,53.6482890991479));
#7805=CARTESIAN_POINT('',(6.70597463025744,-6.5,52.4431278173869));
#7806=CARTESIAN_POINT('',(6.70597463025744,-4.5,52.4431278173869));
#7807=CARTESIAN_POINT('',(19.1306748574635,-6.5,57.9749607648985));
#7808=CARTESIAN_POINT('',(6.70597463025744,-6.5,52.4431278173869));
#7809=CARTESIAN_POINT('',(19.1306748574635,-4.5,57.9749607648985));
#7810=CARTESIAN_POINT('Origin',(0.,-4.5,48.6364583401654));
#7811=CARTESIAN_POINT('',(21.2750522452644,-2.5,49.3864583401654));
#7812=CARTESIAN_POINT('Origin',(0.,-2.5,48.6364583401654));
#7813=CARTESIAN_POINT('',(21.2750522452644,-6.5,49.3864583401654));
#7814=CARTESIAN_POINT('',(21.2750522452644,-4.5,49.3864583401654));
#7815=CARTESIAN_POINT('Origin',(0.,-6.5,48.6364583401654));
#7816=CARTESIAN_POINT('Origin',(0.,-4.5,48.6364583401654));
#7817=CARTESIAN_POINT('',(14.7931472282982,-6.5,63.9450553732257));
#7818=CARTESIAN_POINT('Origin',(0.,-6.5,48.6364583401654));
#7819=CARTESIAN_POINT('',(14.7931472282982,-2.5,63.9450553732257));
#7820=CARTESIAN_POINT('',(14.7931472282982,-4.5,63.9450553732257));
#7821=CARTESIAN_POINT('Origin',(0.,-2.5,48.6364583401654));
#7822=CARTESIAN_POINT('Origin',(0.,-4.5,48.6364583401654));
#7823=CARTESIAN_POINT('',(7.67452462700238,-6.5,49.3864583401654));
#7824=CARTESIAN_POINT('Origin',(0.,-6.5,48.6364583401654));
#7825=CARTESIAN_POINT('',(7.67452462700238,-2.5,49.3864583401654));
#7826=CARTESIAN_POINT('',(7.67452462700238,-4.5,49.3864583401654));
#7827=CARTESIAN_POINT('Origin',(0.,-2.5,48.6364583401654));
#7828=CARTESIAN_POINT('Origin',(0.,-4.5,48.6364583401654));
#7829=CARTESIAN_POINT('',(5.69261793629013,-2.5,53.8378936499519));
#7830=CARTESIAN_POINT('Origin',(0.,-2.5,48.6364583401654));
#7831=CARTESIAN_POINT('',(5.69261793629014,-6.5,53.8378936499519));
#7832=CARTESIAN_POINT('',(5.69261793629013,-4.5,53.8378936499519));
#7833=CARTESIAN_POINT('Origin',(0.,-6.5,48.6364583401654));
#7834=CARTESIAN_POINT('Origin',(-7.35088408256156,-4.5,50.9656924321383));
#7835=CARTESIAN_POINT('',(-3.59747515722412,-2.5,50.167880736427));
#7836=CARTESIAN_POINT('',(-20.6542075410784,-6.5,53.7934011252648));
#7837=CARTESIAN_POINT('Origin',(-20.9660750773051,-4.5,52.3261797241641));
#7838=CARTESIAN_POINT('',(-7.66275161878819,-2.5,49.4984710310376));
#7839=CARTESIAN_POINT('',(-20.9660750773051,-2.5,52.3261797241641));
#7840=CARTESIAN_POINT('',(-10.5610044227092,-2.5,50.1145136818896));
#7841=CARTESIAN_POINT('',(-7.6627516187882,-6.5,49.4984710310376));
#7842=CARTESIAN_POINT('',(-7.66275161878819,-4.5,49.4984710310376));
#7843=CARTESIAN_POINT('',(-20.9660750773051,-6.5,52.3261797241641));
#7844=CARTESIAN_POINT('',(-7.6627516187882,-6.5,49.4984710310376));
#7845=CARTESIAN_POINT('',(-20.9660750773051,-4.5,52.3261797241641));
#7846=CARTESIAN_POINT('Origin',(0.,-4.5,48.6364583401654));
#7847=CARTESIAN_POINT('',(-20.9660750773051,-6.5,44.9467369561667));
#7848=CARTESIAN_POINT('Origin',(0.,-6.5,48.6364583401654));
#7849=CARTESIAN_POINT('',(-20.9660750773051,-2.5,44.9467369561667));
#7850=CARTESIAN_POINT('',(-20.9660750773051,-4.5,44.9467369561667));
#7851=CARTESIAN_POINT('Origin',(0.,-2.5,48.6364583401654));
#7852=CARTESIAN_POINT('Origin',(0.,-4.5,48.6364583401654));
#7853=CARTESIAN_POINT('',(-7.6627516187882,-2.5,47.7744456492932));
#7854=CARTESIAN_POINT('Origin',(0.,-2.5,48.6364583401654));
#7855=CARTESIAN_POINT('',(-7.6627516187882,-6.5,47.7744456492932));
#7856=CARTESIAN_POINT('',(-7.6627516187882,-4.5,47.7744456492932));
#7857=CARTESIAN_POINT('Origin',(0.,-6.5,48.6364583401654));
#7858=CARTESIAN_POINT('Origin',(5.69261793629014,-4.5,53.8378936499519));
#7859=CARTESIAN_POINT('',(3.12498827769909,-2.5,50.9862520176741));
#7860=CARTESIAN_POINT('',(14.7931472282982,-6.5,63.9450553732257));
#7861=CARTESIAN_POINT('Origin',(13.6784299900821,-4.5,64.948751282764));
#7862=CARTESIAN_POINT('',(6.56053568548703,-2.5,57.0435287888493));
#7863=CARTESIAN_POINT('',(4.57790069807404,-6.5,54.8415895594902));
#7864=CARTESIAN_POINT('Origin',(-7.6627516187882,-4.5,47.7744456492932));
#7865=CARTESIAN_POINT('',(-3.90934269345076,-2.5,48.5722573450045));
#7866=CARTESIAN_POINT('',(-20.9660750773051,-6.5,44.9467369561667));
#7867=CARTESIAN_POINT('Origin',(-20.6542075410784,-4.5,43.4795155550659));
#7868=CARTESIAN_POINT('',(-7.35088408256156,-2.5,46.3072242481924));
#7869=CARTESIAN_POINT('',(-20.6542075410784,-2.5,43.4795155550659));
#7870=CARTESIAN_POINT('',(-10.2491368864826,-2.5,45.6911815973405));
#7871=CARTESIAN_POINT('',(-7.35088408256156,-6.5,46.3072242481924));
#7872=CARTESIAN_POINT('',(-7.35088408256156,-4.5,46.3072242481924));
#7873=CARTESIAN_POINT('',(-20.6542075410784,-6.5,43.4795155550659));
#7874=CARTESIAN_POINT('',(-7.35088408256156,-6.5,46.3072242481924));
#7875=CARTESIAN_POINT('',(-20.6542075410784,-4.5,43.4795155550659));
#7876=CARTESIAN_POINT('Origin',(0.,-4.5,48.6364583401654));
#7877=CARTESIAN_POINT('',(-17.6527177618531,-6.5,36.7380591344283));
#7878=CARTESIAN_POINT('Origin',(0.,-6.5,48.6364583401654));
#7879=CARTESIAN_POINT('',(-17.6527177618531,-2.5,36.7380591344283));
#7880=CARTESIAN_POINT('',(-17.6527177618531,-4.5,36.7380591344283));
#7881=CARTESIAN_POINT('Origin',(0.,-2.5,48.6364583401654));
#7882=CARTESIAN_POINT('Origin',(0.,-4.5,48.6364583401654));
#7883=CARTESIAN_POINT('',(-6.64965978621333,-2.5,44.7322486918392));
#7884=CARTESIAN_POINT('Origin',(0.,-2.5,48.6364583401654));
#7885=CARTESIAN_POINT('',(-6.64965978621333,-6.5,44.7322486918392));
#7886=CARTESIAN_POINT('',(-6.64965978621333,-4.5,44.7322486918392));
#7887=CARTESIAN_POINT('Origin',(0.,-6.5,48.6364583401654));
#7888=CARTESIAN_POINT('Origin',(-0.0563148440441186,-4.5,56.347337465713));
#7889=CARTESIAN_POINT('',(0.344788288741045,-2.5,52.5310960766646));
#7890=CARTESIAN_POINT('',(-1.47795709561033,-6.5,69.8733599706355));
#7891=CARTESIAN_POINT('Origin',(-2.96973993866275,-4.5,69.7165672757341));
#7892=CARTESIAN_POINT('',(-1.85781568009448,-2.5,59.1373146342244));
#7893=CARTESIAN_POINT('',(-1.54809768709653,-6.5,56.1905447708115));
#7894=CARTESIAN_POINT('Origin',(-1.57645741831176,-4.5,17.3563656672972));
#7895=CARTESIAN_POINT('',(-1.57645741831176,-2.5,17.3563656672972));
#7896=CARTESIAN_POINT('',(-1.97778180513782,-2.5,23.4256497460872));
#7897=CARTESIAN_POINT('',(-2.60270384171029,-2.5,32.8764319351548));
#7898=CARTESIAN_POINT('',(-1.97778180513782,-6.5,23.4256497460872));
#7899=CARTESIAN_POINT('',(-1.97778180513782,-4.5,23.4256497460872));
#7900=CARTESIAN_POINT('',(-1.57645741831176,-6.5,17.3563656672972));
#7901=CARTESIAN_POINT('',(-1.55556094933235,-6.5,17.0403454835185));
#7902=CARTESIAN_POINT('',(-1.57645741831176,-4.5,17.3563656672972));
#7903=CARTESIAN_POINT('Origin',(-1.67601818730369,-4.5,17.3339592456822));
#7904=CARTESIAN_POINT('',(-1.67601818730369,-2.5,17.3339592456822));
#7905=CARTESIAN_POINT('',(2.47414659150376,-2.5,18.267965107099));
#7906=CARTESIAN_POINT('',(-1.67601818730369,-6.5,17.3339592456822));
#7907=CARTESIAN_POINT('',(-0.87670375950466,-6.5,17.5138471297709));
#7908=CARTESIAN_POINT('',(-1.67601818730369,-4.5,17.3339592456822));
#7909=CARTESIAN_POINT('Origin',(-4.29406553618937,-4.5,23.7154332407259));
#7910=CARTESIAN_POINT('',(-4.29406553618937,-2.5,23.7154332407259));
#7911=CARTESIAN_POINT('',(-8.3603183566449,-2.5,33.6268989909746));
#7912=CARTESIAN_POINT('',(-4.29406553618937,-6.5,23.7154332407259));
#7913=CARTESIAN_POINT('',(-1.55556094933235,-6.5,17.0403454835185));
#7914=CARTESIAN_POINT('',(-4.29406553618937,-4.5,23.7154332407259));
#7915=CARTESIAN_POINT('Origin',(0.,-4.5,48.6364583401654));
#7916=CARTESIAN_POINT('',(0.981142563718935,-2.5,23.3672310052103));
#7917=CARTESIAN_POINT('Origin',(0.,-2.5,48.6364583401654));
#7918=CARTESIAN_POINT('',(0.981142563718941,-6.5,23.3672310052103));
#7919=CARTESIAN_POINT('',(0.981142563718935,-4.5,23.3672310052103));
#7920=CARTESIAN_POINT('Origin',(0.,-6.5,48.6364583401654));
#7921=CARTESIAN_POINT('Origin',(0.,-4.5,48.6364583401654));
#7922=CARTESIAN_POINT('',(-7.17618436914824,-6.5,24.3877703604834));
#7923=CARTESIAN_POINT('Origin',(0.,-6.5,48.6364583401654));
#7924=CARTESIAN_POINT('',(-7.17618436914824,-2.5,24.3877703604834));
#7925=CARTESIAN_POINT('',(-7.17618436914824,-4.5,24.3877703604834));
#7926=CARTESIAN_POINT('Origin',(0.,-2.5,48.6364583401654));
#7927=CARTESIAN_POINT('Origin',(-8.04550499793289,-4.5,18.3676746688116));
#7928=CARTESIAN_POINT('',(-8.04550499793289,-2.5,18.3676746688116));
#7929=CARTESIAN_POINT('',(-5.82252225538787,-2.5,33.7619588810307));
#7930=CARTESIAN_POINT('',(-8.04550499793289,-6.5,18.3676746688116));
#7931=CARTESIAN_POINT('',(-8.09076945767883,-6.5,18.0542156640675));
#7932=CARTESIAN_POINT('',(-8.04550499793289,-4.5,18.3676746688116));
#7933=CARTESIAN_POINT('Origin',(-8.14754868225271,-4.5,18.3664577290881));
#7934=CARTESIAN_POINT('',(-8.14754868225271,-2.5,18.3664577290881));
#7935=CARTESIAN_POINT('',(-3.8938842233314,-2.5,18.4171855451701));
#7936=CARTESIAN_POINT('',(-8.14754868225271,-6.5,18.3664577290881));
#7937=CARTESIAN_POINT('',(-7.32830039833065,-6.5,18.3762278171319));
#7938=CARTESIAN_POINT('',(-8.14754868225271,-4.5,18.3664577290881));
#7939=CARTESIAN_POINT('Origin',(-9.38160236695364,-4.5,25.1528038574331));
#7940=CARTESIAN_POINT('',(-9.38160236695365,-2.5,25.1528038574331));
#7941=CARTESIAN_POINT('',(-11.2982882046428,-2.5,35.6931017999876));
#7942=CARTESIAN_POINT('',(-9.38160236695364,-6.5,25.1528038574331));
#7943=CARTESIAN_POINT('',(-8.09076945767883,-6.5,18.0542156640675));
#7944=CARTESIAN_POINT('',(-9.38160236695365,-4.5,25.1528038574331));
#7945=CARTESIAN_POINT('Origin',(0.,-4.5,48.6364583401654));
#7946=CARTESIAN_POINT('',(-12.0609532410738,-6.5,26.4096749977063));
#7947=CARTESIAN_POINT('Origin',(0.,-6.5,48.6364583401654));
#7948=CARTESIAN_POINT('',(-12.0609532410738,-2.5,26.4096749977063));
#7949=CARTESIAN_POINT('',(-12.0609532410738,-4.5,26.4096749977063));
#7950=CARTESIAN_POINT('Origin',(0.,-2.5,48.6364583401654));
#7951=CARTESIAN_POINT('Origin',(-19.6613580057765,-4.5,24.2569502035424));
#7952=CARTESIAN_POINT('',(-19.6613580057765,-2.5,24.2569502035424));
#7953=CARTESIAN_POINT('',(-16.4186005814896,-2.5,29.4029967229345));
#7954=CARTESIAN_POINT('',(-11.3691427358738,-2.5,37.4161600809562));
#7955=CARTESIAN_POINT('',(-16.4186005814896,-6.5,29.4029967229345));
#7956=CARTESIAN_POINT('',(-16.4186005814896,-4.5,29.4029967229345));
#7957=CARTESIAN_POINT('',(-19.6613580057765,-6.5,24.2569502035424));
#7958=CARTESIAN_POINT('',(-19.8302044107015,-6.5,23.989001868009));
#7959=CARTESIAN_POINT('',(-19.6613580057765,-4.5,24.2569502035424));
#7960=CARTESIAN_POINT('Origin',(-19.7550745240459,-4.5,24.2973433793931));
#7961=CARTESIAN_POINT('',(-19.7550745240459,-2.5,24.2973433793931));
#7962=CARTESIAN_POINT('',(-15.8485258176388,-2.5,22.6135643425585));
#7963=CARTESIAN_POINT('',(-19.7550745240459,-6.5,24.2973433793931));
#7964=CARTESIAN_POINT('',(-19.0026801227739,-6.5,23.9730505020982));
#7965=CARTESIAN_POINT('',(-19.7550745240459,-4.5,24.2973433793931));
#7966=CARTESIAN_POINT('Origin',(-18.1221830191981,-4.5,30.9989139120237));
#7967=CARTESIAN_POINT('',(-18.1221830191981,-2.5,30.9989139120237));
#7968=CARTESIAN_POINT('',(-15.5860372577735,-2.5,41.4075415830966));
#7969=CARTESIAN_POINT('',(-18.1221830191981,-6.5,30.9989139120237));
#7970=CARTESIAN_POINT('',(-19.8302044107015,-6.5,23.989001868009));
#7971=CARTESIAN_POINT('',(-18.1221830191981,-4.5,30.9989139120237));
#7972=CARTESIAN_POINT('Origin',(0.,-4.5,48.6364583401654));
#7973=CARTESIAN_POINT('',(-14.0591181563592,-2.5,27.6165228621123));
#7974=CARTESIAN_POINT('Origin',(0.,-2.5,48.6364583401654));
#7975=CARTESIAN_POINT('',(-14.0591181563592,-6.5,27.6165228621123));
#7976=CARTESIAN_POINT('',(-14.0591181563592,-4.5,27.6165228621123));
#7977=CARTESIAN_POINT('Origin',(0.,-6.5,48.6364583401654));
#7978=CARTESIAN_POINT('Origin',(0.,-4.5,48.6364583401654));
#7979=CARTESIAN_POINT('',(-20.0586762913076,-6.5,33.2369130132242));
#7980=CARTESIAN_POINT('Origin',(0.,-6.5,48.6364583401654));
#7981=CARTESIAN_POINT('',(-20.0586762913077,-2.5,33.2369130132242));
#7982=CARTESIAN_POINT('',(-20.0586762913077,-4.5,33.2369130132242));
#7983=CARTESIAN_POINT('Origin',(0.,-2.5,48.6364583401654));
#7984=CARTESIAN_POINT('Origin',(-27.8775835965913,-4.5,34.3616641759737));
#7985=CARTESIAN_POINT('',(-27.8775835965913,-2.5,34.3616641759737));
#7986=CARTESIAN_POINT('',(-22.8220915949877,-2.5,37.7438633295183));
#7987=CARTESIAN_POINT('',(-14.9499351519079,-2.5,43.0104527831085));
#7988=CARTESIAN_POINT('',(-22.8220915949877,-6.5,37.7438633295183));
#7989=CARTESIAN_POINT('',(-22.8220915949877,-4.5,37.7438633295183));
#7990=CARTESIAN_POINT('',(-27.8775835965913,-6.5,34.3616641759737));
#7991=CARTESIAN_POINT('',(-28.1408168693625,-6.5,34.1855572110988));
#7992=CARTESIAN_POINT('',(-27.8775835965913,-4.5,34.3616641759737));
#7993=CARTESIAN_POINT('Origin',(-27.9467685114137,-4.5,34.4366831203335));
#7994=CARTESIAN_POINT('',(-27.9467685114137,-2.5,34.4366831203335));
#7995=CARTESIAN_POINT('',(-25.0628133187395,-2.5,31.3095379227032));
#7996=CARTESIAN_POINT('',(-27.9467685114137,-6.5,34.4366831203335));
#7997=CARTESIAN_POINT('',(-27.3913238200603,-6.5,33.8344004622925));
#7998=CARTESIAN_POINT('',(-27.9467685114137,-4.5,34.4366831203335));
#7999=CARTESIAN_POINT('Origin',(-23.7292735925589,-4.5,39.8947156303009));
#8000=CARTESIAN_POINT('',(-23.7292735925589,-2.5,39.8947156303009));
#8001=CARTESIAN_POINT('',(-17.1788188743319,-2.5,48.3719267461499));
#8002=CARTESIAN_POINT('',(-23.7292735925589,-6.5,39.8947156303009));
#8003=CARTESIAN_POINT('',(-28.1408168693625,-6.5,34.1855572110988));
#8004=CARTESIAN_POINT('',(-23.7292735925589,-4.5,39.8947156303009));
#8005=CARTESIAN_POINT('Origin',(0.,-4.5,48.6364583401654));
#8006=CARTESIAN_POINT('',(-21.3932215242158,-2.5,35.152150287773));
#8007=CARTESIAN_POINT('Origin',(0.,-2.5,48.6364583401654));
#8008=CARTESIAN_POINT('',(-21.3932215242158,-6.5,35.152150287773));
#8009=CARTESIAN_POINT('',(-21.3932215242158,-4.5,35.152150287773));
#8010=CARTESIAN_POINT('Origin',(0.,-6.5,48.6364583401654));
#8011=CARTESIAN_POINT('Origin',(0.,-4.5,48.6364583401654));
#8012=CARTESIAN_POINT('',(-24.5880719834211,-6.5,42.7268723162475));
#8013=CARTESIAN_POINT('Origin',(0.,-6.5,48.6364583401654));
#8014=CARTESIAN_POINT('',(-24.5880719834211,-2.5,42.7268723162476));
#8015=CARTESIAN_POINT('',(-24.5880719834211,-4.5,42.7268723162476));
#8016=CARTESIAN_POINT('Origin',(0.,-2.5,48.6364583401654));
#8017=CARTESIAN_POINT('Origin',(-24.3004949185092,-4.5,28.8775271360116));
#8018=CARTESIAN_POINT('',(-24.3004949185092,-2.5,28.8775271360116));
#8019=CARTESIAN_POINT('',(-13.4535308720469,-2.5,40.0251282077662));
#8020=CARTESIAN_POINT('',(-24.3004949185092,-6.5,28.8775271360116));
#8021=CARTESIAN_POINT('',(-24.5213612158718,-6.5,28.6505392560254));
#8022=CARTESIAN_POINT('',(-24.3004949185092,-4.5,28.8775271360116));
#8023=CARTESIAN_POINT('Origin',(-24.383765292515,-4.5,28.936522383827));
#8024=CARTESIAN_POINT('',(-24.383765292515,-2.5,28.936522383827));
#8025=CARTESIAN_POINT('',(-20.912661394705,-2.5,26.4773208119702));
#8026=CARTESIAN_POINT('',(-24.383765292515,-6.5,28.936522383827));
#8027=CARTESIAN_POINT('',(-23.7152367945438,-6.5,28.4628844918356));
#8028=CARTESIAN_POINT('',(-24.383765292515,-4.5,28.936522383827));
#8029=CARTESIAN_POINT('Origin',(-21.3932215242158,-4.5,35.152150287773));
#8030=CARTESIAN_POINT('',(-16.7484212543818,-2.5,44.8060301177464));
#8031=CARTESIAN_POINT('',(-24.5213612158718,-6.5,28.6505392560254));
#8032=CARTESIAN_POINT('Origin',(4.96148891517159,-4.5,17.7121468141248));
#8033=CARTESIAN_POINT('',(4.96148891517159,-2.5,17.7121468141248));
#8034=CARTESIAN_POINT('',(0.730865219008715,-2.5,32.679693768175));
#8035=CARTESIAN_POINT('',(4.96148891517159,-6.5,17.7121468141248));
#8036=CARTESIAN_POINT('',(5.04763303690956,-6.5,17.4073770497759));
#8037=CARTESIAN_POINT('',(4.96148891517159,-4.5,17.7121468141248));
#8038=CARTESIAN_POINT('Origin',(4.86876234485807,-4.5,17.6695301787609));
#8039=CARTESIAN_POINT('',(4.86876234485807,-2.5,17.6695301787609));
#8040=CARTESIAN_POINT('',(8.73404532801765,-2.5,19.4459935475112));
#8041=CARTESIAN_POINT('',(4.86876234485807,-6.5,17.6695301787609));
#8042=CARTESIAN_POINT('',(5.61320904050308,-6.5,18.0116738951621));
#8043=CARTESIAN_POINT('',(4.86876234485807,-4.5,17.6695301787609));
#8044=CARTESIAN_POINT('Origin',(0.981142563718943,-4.5,23.3672310052103));
#8045=CARTESIAN_POINT('',(-5.05696247920324,-2.5,32.216685949378));
#8046=CARTESIAN_POINT('',(5.04763303690956,-6.5,17.4073770497759));
#8047=CARTESIAN_POINT('Origin',(-14.162925402528,-4.5,20.7018747625031));
#8048=CARTESIAN_POINT('',(-14.162925402528,-2.5,20.7018747625031));
#8049=CARTESIAN_POINT('',(-8.78786850694337,-2.5,35.2975728290382));
#8050=CARTESIAN_POINT('',(-14.162925402528,-6.5,20.7018747625031));
#8051=CARTESIAN_POINT('',(-14.2723725169055,-6.5,20.4046765994439));
#8052=CARTESIAN_POINT('',(-14.162925402528,-4.5,20.7018747625031));
#8053=CARTESIAN_POINT('Origin',(-14.262992203511,-4.5,20.7219004907765));
#8054=CARTESIAN_POINT('',(-14.262992203511,-2.5,20.7219004907765));
#8055=CARTESIAN_POINT('',(-10.0917336126774,-2.5,19.8871332125418));
#8056=CARTESIAN_POINT('',(-14.262992203511,-6.5,20.7219004907765));
#8057=CARTESIAN_POINT('',(-13.4596151446628,-6.5,20.5611257830457));
#8058=CARTESIAN_POINT('',(-14.262992203511,-4.5,20.7219004907765));
#8059=CARTESIAN_POINT('Origin',(-14.0591181563592,-4.5,27.6165228621123));
#8060=CARTESIAN_POINT('',(-13.7424686428958,-2.5,38.3249913989219));
#8061=CARTESIAN_POINT('',(-14.2723725169055,-6.5,20.4046765994439));
#8062=CARTESIAN_POINT('Origin',(-30.2362881000144,-4.5,40.4696782189731));
#8063=CARTESIAN_POINT('',(-30.2362881000144,-2.5,40.4696782189731));
#8064=CARTESIAN_POINT('',(-15.7929555278825,-2.5,46.2416607978642));
#8065=CARTESIAN_POINT('',(-30.2362881000144,-6.5,40.4696782189731));
#8066=CARTESIAN_POINT('',(-30.5303837910408,-6.5,40.3521488886295));
#8067=CARTESIAN_POINT('',(-30.2362881000144,-4.5,40.4696782189731));
#8068=CARTESIAN_POINT('Origin',(-30.2883638428897,-4.5,40.557442172028));
#8069=CARTESIAN_POINT('',(-30.2883638428897,-2.5,40.557442172028));
#8070=CARTESIAN_POINT('',(-28.1176000360236,-2.5,36.8990245994682));
#8071=CARTESIAN_POINT('',(-30.2883638428897,-6.5,40.557442172028));
#8072=CARTESIAN_POINT('',(-29.8702785564856,-6.5,39.8528373901666));
#8073=CARTESIAN_POINT('',(-30.2883638428897,-4.5,40.557442172028));
#8074=CARTESIAN_POINT('Origin',(-25.0282425392193,-4.5,45.0193370767853));
#8075=CARTESIAN_POINT('',(-25.0282425392193,-2.5,45.0193370767853));
#8076=CARTESIAN_POINT('',(-16.8584196763548,-2.5,51.9493846745752));
#8077=CARTESIAN_POINT('',(-25.0282425392193,-6.5,45.0193370767853));
#8078=CARTESIAN_POINT('',(-30.5303837910408,-6.5,40.3521488886295));
#8079=CARTESIAN_POINT('',(-25.0282425392193,-4.5,45.0193370767853));
#8080=CARTESIAN_POINT('Origin',(0.,-4.5,48.6364583401654));
#8081=CARTESIAN_POINT('',(-25.2794356395192,-6.5,47.968158569562));
#8082=CARTESIAN_POINT('Origin',(0.,-6.5,48.6364583401654));
#8083=CARTESIAN_POINT('',(-25.2794356395192,-2.5,47.968158569562));
#8084=CARTESIAN_POINT('',(-25.2794356395192,-4.5,47.968158569562));
#8085=CARTESIAN_POINT('Origin',(0.,-2.5,48.6364583401654));
#8086=CARTESIAN_POINT('Origin',(-6.64965978621333,-4.5,44.7322486918392));
#8087=CARTESIAN_POINT('',(-3.54524936271634,-2.5,46.9877348888929));
#8088=CARTESIAN_POINT('',(-17.6527177618531,-6.5,36.7380591344283));
#8089=CARTESIAN_POINT('Origin',(-16.7710398834144,-4.5,35.5245336428659));
#8090=CARTESIAN_POINT('',(-5.76798190777462,-2.5,43.5187232002768));
#8091=CARTESIAN_POINT('',(-16.7710398834144,-2.5,35.5245336428659));
#8092=CARTESIAN_POINT('',(-8.16510047209754,-2.5,41.777114618625));
#8093=CARTESIAN_POINT('',(-5.76798190777462,-6.5,43.5187232002768));
#8094=CARTESIAN_POINT('',(-5.76798190777462,-4.5,43.5187232002768));
#8095=CARTESIAN_POINT('',(-16.7710398834144,-6.5,35.5245336428659));
#8096=CARTESIAN_POINT('',(-5.76798190777462,-6.5,43.5187232002768));
#8097=CARTESIAN_POINT('',(-16.7710398834144,-4.5,35.5245336428659));
#8098=CARTESIAN_POINT('Origin',(0.,-4.5,48.6364583401654));
#8099=CARTESIAN_POINT('',(-11.2870451754705,-6.5,30.5867226289253));
#8100=CARTESIAN_POINT('Origin',(0.,-6.5,48.6364583401654));
#8101=CARTESIAN_POINT('',(-11.2870451754705,-2.5,30.5867226289253));
#8102=CARTESIAN_POINT('',(-11.2870451754705,-4.5,30.5867226289253));
#8103=CARTESIAN_POINT('Origin',(0.,-2.5,48.6364583401654));
#8104=CARTESIAN_POINT('Origin',(0.,-4.5,48.6364583401654));
#8105=CARTESIAN_POINT('',(-4.48678136633952,-2.5,42.365125051212));
#8106=CARTESIAN_POINT('Origin',(0.,-2.5,48.6364583401654));
#8107=CARTESIAN_POINT('',(-4.48678136633952,-6.5,42.365125051212));
#8108=CARTESIAN_POINT('',(-4.48678136633952,-4.5,42.365125051212));
#8109=CARTESIAN_POINT('Origin',(0.,-6.5,48.6364583401654));
#8110=CARTESIAN_POINT('Origin',(-1.54809768709653,-4.5,41.0823719095192));
#8111=CARTESIAN_POINT('',(-2.96973993866273,-2.5,27.5563494045967));
#8112=CARTESIAN_POINT('',(-1.54809768709653,-2.5,41.0823719095192));
#8113=CARTESIAN_POINT('',(-1.14699455431137,-2.5,44.8986132985677));
#8114=CARTESIAN_POINT('',(-2.96973993866273,-6.5,27.5563494045967));
#8115=CARTESIAN_POINT('',(-2.96973993866273,-4.5,27.5563494045967));
#8116=CARTESIAN_POINT('',(-1.54809768709653,-6.5,41.0823719095192));
#8117=CARTESIAN_POINT('',(-2.96973993866273,-6.5,27.5563494045967));
#8118=CARTESIAN_POINT('',(-1.54809768709653,-4.5,41.0823719095192));
#8119=CARTESIAN_POINT('Origin',(-1.47795709561032,-4.5,27.3995567096953));
#8120=CARTESIAN_POINT('',(-0.366032837042061,-2.5,37.978809351205));
#8121=CARTESIAN_POINT('',(-0.0563148440441186,-6.5,40.9255792146178));
#8122=CARTESIAN_POINT('Origin',(0.,-4.5,48.6364583401654));
#8123=CARTESIAN_POINT('',(-9.98800706979387,-2.5,29.8367226289253));
#8124=CARTESIAN_POINT('Origin',(0.,-2.5,48.6364583401654));
#8125=CARTESIAN_POINT('',(-9.98800706979387,-6.5,29.8367226289253));
#8126=CARTESIAN_POINT('',(-9.98800706979387,-4.5,29.8367226289253));
#8127=CARTESIAN_POINT('Origin',(0.,-6.5,48.6364583401654));
#8128=CARTESIAN_POINT('Origin',(0.,-4.5,48.6364583401654));
#8129=CARTESIAN_POINT('',(-3.18774326066286,-6.5,41.615125051212));
#8130=CARTESIAN_POINT('Origin',(0.,-6.5,48.6364583401654));
#8131=CARTESIAN_POINT('',(-3.18774326066286,-2.5,41.615125051212));
#8132=CARTESIAN_POINT('',(-3.18774326066286,-4.5,41.615125051212));
#8133=CARTESIAN_POINT('Origin',(0.,-2.5,48.6364583401654));
#8134=CARTESIAN_POINT('Origin',(-4.48678136633952,-4.5,42.365125051212));
#8135=CARTESIAN_POINT('',(-2.56815020958893,-2.5,45.6882916956887));
#8136=CARTESIAN_POINT('',(-11.2870451754705,-6.5,30.5867226289253));
#8137=CARTESIAN_POINT('Origin',(-9.98800706979387,-4.5,29.8367226289253));
#8138=CARTESIAN_POINT('',(-4.66924400847777,-2.5,39.0490904845453));
#8139=CARTESIAN_POINT('',(-3.18774326066286,-6.5,41.615125051212));
#8140=CARTESIAN_POINT('Origin',(-29.2619838336808,-4.5,59.8018386620522));
#8141=CARTESIAN_POINT('',(-29.2619838336808,-2.5,59.8018386620522));
#8142=CARTESIAN_POINT('',(-23.3657356055148,-2.5,58.3080089112559));
#8143=CARTESIAN_POINT('',(-14.1843960910556,-2.5,55.9818927797566));
#8144=CARTESIAN_POINT('',(-23.3657356055148,-6.5,58.3080089112559));
#8145=CARTESIAN_POINT('',(-23.3657356055148,-4.5,58.3080089112559));
#8146=CARTESIAN_POINT('',(-29.2619838336808,-6.5,59.8018386620522));
#8147=CARTESIAN_POINT('',(-29.5689942527814,-6.5,59.8796205464148));
#8148=CARTESIAN_POINT('',(-29.2619838336808,-4.5,59.8018386620522));
#8149=CARTESIAN_POINT('Origin',(-29.2525276373731,-4.5,59.9034505452315));
#8150=CARTESIAN_POINT('',(-29.2525276373731,-2.5,59.9034505452315));
#8151=CARTESIAN_POINT('',(-29.6467067227226,-2.5,55.6677856046244));
#8152=CARTESIAN_POINT('',(-29.2525276373731,-6.5,59.9034505452315));
#8153=CARTESIAN_POINT('',(-29.3284458350469,-6.5,59.0876689368389));
#8154=CARTESIAN_POINT('',(-29.2525276373731,-4.5,59.9034505452315));
#8155=CARTESIAN_POINT('Origin',(-22.3743640879348,-4.5,60.4213776227282));
#8156=CARTESIAN_POINT('',(-22.3743640879347,-2.5,60.4213776227282));
#8157=CARTESIAN_POINT('',(-11.6914587751786,-2.5,61.2258025085338));
#8158=CARTESIAN_POINT('',(-22.3743640879347,-6.5,60.4213776227282));
#8159=CARTESIAN_POINT('',(-29.5689942527814,-6.5,59.8796205464148));
#8160=CARTESIAN_POINT('',(-22.3743640879347,-4.5,60.4213776227282));
#8161=CARTESIAN_POINT('Origin',(0.,-4.5,48.6364583401654));
#8162=CARTESIAN_POINT('',(-24.3356530447464,-2.5,55.511956992751));
#8163=CARTESIAN_POINT('Origin',(0.,-2.5,48.6364583401654));
#8164=CARTESIAN_POINT('',(-24.3356530447464,-6.5,55.5119569927511));
#8165=CARTESIAN_POINT('',(-24.3356530447464,-4.5,55.511956992751));
#8166=CARTESIAN_POINT('Origin',(0.,-6.5,48.6364583401654));
#8167=CARTESIAN_POINT('Origin',(0.,-4.5,48.6364583401654));
#8168=CARTESIAN_POINT('',(-20.8443097898499,-6.5,62.9546719235965));
#8169=CARTESIAN_POINT('Origin',(0.,-6.5,48.6364583401654));
#8170=CARTESIAN_POINT('',(-20.8443097898499,-2.5,62.9546719235965));
#8171=CARTESIAN_POINT('',(-20.8443097898499,-4.5,62.9546719235965));
#8172=CARTESIAN_POINT('Origin',(0.,-2.5,48.6364583401654));
#8173=CARTESIAN_POINT('Origin',(-26.3011261782795,-4.5,65.6417568488419));
#8174=CARTESIAN_POINT('',(-26.3011261782795,-2.5,65.6417568488419));
#8175=CARTESIAN_POINT('',(-12.3472313101976,-2.5,58.7704791881192));
#8176=CARTESIAN_POINT('',(-26.3011261782795,-6.5,65.6417568488419));
#8177=CARTESIAN_POINT('',(-26.5852559200301,-6.5,65.7816700677457));
#8178=CARTESIAN_POINT('',(-26.3011261782795,-4.5,65.6417568488419));
#8179=CARTESIAN_POINT('Origin',(-26.27075032411,-4.5,65.7391822148167));
#8180=CARTESIAN_POINT('',(-26.27075032411,-2.5,65.7391822148167));
#8181=CARTESIAN_POINT('',(-27.5369599102432,-2.5,61.6780311557697));
#8182=CARTESIAN_POINT('',(-26.27075032411,-6.5,65.7391822148167));
#8183=CARTESIAN_POINT('',(-26.5146200605557,-6.5,64.957011672687));
#8184=CARTESIAN_POINT('',(-26.27075032411,-4.5,65.7391822148167));
#8185=CARTESIAN_POINT('Origin',(-19.4352080563696,-4.5,64.8157407297404));
#8186=CARTESIAN_POINT('',(-19.4352080563695,-2.5,64.8157407297404));
#8187=CARTESIAN_POINT('',(-8.81850051768697,-2.5,63.3814860953406));
#8188=CARTESIAN_POINT('',(-19.4352080563696,-6.5,64.8157407297404));
#8189=CARTESIAN_POINT('',(-26.5852559200301,-6.5,65.7816700677457));
#8190=CARTESIAN_POINT('',(-19.4352080563695,-4.5,64.8157407297404));
#8191=CARTESIAN_POINT('Origin',(0.,-4.5,48.6364583401654));
#8192=CARTESIAN_POINT('',(-17.4118876142729,-6.5,66.9755602959296));
#8193=CARTESIAN_POINT('Origin',(0.,-6.5,48.6364583401654));
#8194=CARTESIAN_POINT('',(-17.4118876142729,-2.5,66.9755602959296));
#8195=CARTESIAN_POINT('',(-17.4118876142729,-4.5,66.9755602959296));
#8196=CARTESIAN_POINT('Origin',(0.,-2.5,48.6364583401654));
#8197=CARTESIAN_POINT('Origin',(-11.2825943751967,-4.5,77.8534479143798));
#8198=CARTESIAN_POINT('',(-11.2825943751967,-2.5,77.8534479143798));
#8199=CARTESIAN_POINT('',(-8.44736607249009,-2.5,72.4721143469408));
#8200=CARTESIAN_POINT('',(-4.03249196257662,-2.5,64.092573898288));
#8201=CARTESIAN_POINT('',(-8.44736607249009,-6.5,72.4721143469408));
#8202=CARTESIAN_POINT('',(-8.44736607249009,-4.5,72.4721143469408));
#8203=CARTESIAN_POINT('',(-11.2825943751967,-6.5,77.8534479143798));
#8204=CARTESIAN_POINT('',(-11.4302212382079,-6.5,78.1336473581494));
#8205=CARTESIAN_POINT('',(-11.2825943751967,-4.5,77.8534479143798));
#8206=CARTESIAN_POINT('Origin',(-11.2007545996357,-4.5,77.91441221203));
#8207=CARTESIAN_POINT('',(-11.2007545996357,-2.5,77.91441221203));
#8208=CARTESIAN_POINT('',(-14.6122243730978,-2.5,75.3731313095776));
#8209=CARTESIAN_POINT('',(-11.2007545996357,-6.5,77.91441221203));
#8210=CARTESIAN_POINT('',(-11.8577976702754,-6.5,77.4249659855108));
#8211=CARTESIAN_POINT('',(-11.2007545996357,-4.5,77.91441221203));
#8212=CARTESIAN_POINT('Origin',(-6.21347002554836,-4.5,73.1495014208928));
#8213=CARTESIAN_POINT('',(-6.21347002554835,-2.5,73.1495014208928));
#8214=CARTESIAN_POINT('',(1.53259307542215,-2.5,65.7488209282624));
#8215=CARTESIAN_POINT('',(-6.21347002554836,-6.5,73.1495014208928));
#8216=CARTESIAN_POINT('',(-11.4302212382079,-6.5,78.1336473581494));
#8217=CARTESIAN_POINT('',(-6.21347002554835,-4.5,73.1495014208928));
#8218=CARTESIAN_POINT('Origin',(0.,-4.5,48.6364583401654));
#8219=CARTESIAN_POINT('',(-11.1742390317241,-2.5,71.3219795574061));
#8220=CARTESIAN_POINT('Origin',(0.,-2.5,48.6364583401654));
#8221=CARTESIAN_POINT('',(-11.1742390317241,-6.5,71.3219795574061));
#8222=CARTESIAN_POINT('',(-11.1742390317241,-4.5,71.3219795574061));
#8223=CARTESIAN_POINT('Origin',(0.,-6.5,48.6364583401654));
#8224=CARTESIAN_POINT('Origin',(0.,-4.5,48.6364583401654));
#8225=CARTESIAN_POINT('',(-3.30705931420718,-6.5,73.707554238197));
#8226=CARTESIAN_POINT('Origin',(0.,-6.5,48.6364583401654));
#8227=CARTESIAN_POINT('',(-3.30705931420718,-2.5,73.707554238197));
#8228=CARTESIAN_POINT('',(-3.30705931420718,-4.5,73.707554238197));
#8229=CARTESIAN_POINT('Origin',(0.,-2.5,48.6364583401654));
#8230=CARTESIAN_POINT('Origin',(-22.1907831020815,-4.5,70.7384618903268));
#8231=CARTESIAN_POINT('',(-22.1907831020815,-2.5,70.7384618903268));
#8232=CARTESIAN_POINT('',(-9.97043327249461,-2.5,61.1161602569989));
#8233=CARTESIAN_POINT('',(-22.1907831020815,-6.5,70.7384618903268));
#8234=CARTESIAN_POINT('',(-22.439614333362,-6.5,70.9343915647275));
#8235=CARTESIAN_POINT('',(-22.1907831020815,-4.5,70.7384618903268));
#8236=CARTESIAN_POINT('Origin',(-22.140815160637,-4.5,70.8274427831053));
#8237=CARTESIAN_POINT('',(-22.140815160637,-2.5,70.8274427831053));
#8238=CARTESIAN_POINT('',(-24.2237158126922,-2.5,67.1182973944635));
#8239=CARTESIAN_POINT('',(-22.140815160637,-6.5,70.8274427831053));
#8240=CARTESIAN_POINT('',(-22.541978158155,-6.5,70.1130679132001));
#8241=CARTESIAN_POINT('',(-22.140815160637,-4.5,70.8274427831053));
#8242=CARTESIAN_POINT('Origin',(-15.6466401722657,-4.5,68.5029915595176));
#8243=CARTESIAN_POINT('',(-15.6466401722657,-2.5,68.5029915595176));
#8244=CARTESIAN_POINT('',(-5.56013147171207,-2.5,64.892741214753));
#8245=CARTESIAN_POINT('',(-15.6466401722657,-6.5,68.5029915595176));
#8246=CARTESIAN_POINT('',(-22.439614333362,-6.5,70.9343915647275));
#8247=CARTESIAN_POINT('',(-15.6466401722657,-4.5,68.5029915595176));
#8248=CARTESIAN_POINT('Origin',(0.,-4.5,48.6364583401654));
#8249=CARTESIAN_POINT('',(-13.2184823984455,-6.5,70.1949419120211));
#8250=CARTESIAN_POINT('Origin',(0.,-6.5,48.6364583401654));
#8251=CARTESIAN_POINT('',(-13.2184823984455,-2.5,70.1949419120211));
#8252=CARTESIAN_POINT('',(-13.2184823984455,-4.5,70.1949419120211));
#8253=CARTESIAN_POINT('Origin',(0.,-2.5,48.6364583401654));
#8254=CARTESIAN_POINT('Origin',(-31.2735217236592,-4.5,46.9346197418275));
#8255=CARTESIAN_POINT('',(-31.2735217236592,-2.5,46.9346197418275));
#8256=CARTESIAN_POINT('',(-15.94574796428,-2.5,49.577532956732));
#8257=CARTESIAN_POINT('',(-31.2735217236592,-6.5,46.9346197418275));
#8258=CARTESIAN_POINT('',(-31.5856264400152,-6.5,46.8808046417196));
#8259=CARTESIAN_POINT('',(-31.2735217236592,-4.5,46.9346197418275));
#8260=CARTESIAN_POINT('Origin',(-31.3062123347366,-4.5,47.0312929976909));
#8261=CARTESIAN_POINT('',(-31.3062123347366,-2.5,47.0312929976909));
#8262=CARTESIAN_POINT('',(-29.943512708519,-2.5,43.0014934531576));
#8263=CARTESIAN_POINT('',(-31.3062123347366,-6.5,47.0312929976909));
#8264=CARTESIAN_POINT('',(-31.0437587864934,-6.5,46.2551607020453));
#8265=CARTESIAN_POINT('',(-31.3062123347366,-4.5,47.0312929976909));
#8266=CARTESIAN_POINT('Origin',(-25.2333571880834,-4.5,50.302044079353));
#8267=CARTESIAN_POINT('',(-25.2333571880834,-2.5,50.302044079353));
#8268=CARTESIAN_POINT('',(-15.8012266428482,-2.5,55.3820518250025));
#8269=CARTESIAN_POINT('',(-25.2333571880834,-6.5,50.302044079353));
#8270=CARTESIAN_POINT('',(-31.5856264400152,-6.5,46.8808046417196));
#8271=CARTESIAN_POINT('',(-25.2333571880834,-4.5,50.302044079353));
#8272=CARTESIAN_POINT('Origin',(0.,-4.5,48.6364583401654));
#8273=CARTESIAN_POINT('',(-24.8659666539797,-6.5,53.2386527297099));
#8274=CARTESIAN_POINT('Origin',(0.,-6.5,48.6364583401654));
#8275=CARTESIAN_POINT('',(-24.8659666539797,-2.5,53.2386527297099));
#8276=CARTESIAN_POINT('',(-24.8659666539797,-4.5,53.2386527297099));
#8277=CARTESIAN_POINT('Origin',(0.,-2.5,48.6364583401654));
#8278=CARTESIAN_POINT('Origin',(-4.9614889151716,-4.5,79.5607698662059));
#8279=CARTESIAN_POINT('',(-4.9614889151716,-2.5,79.5607698662059));
#8280=CARTESIAN_POINT('',(-0.730865219008718,-2.5,64.5932229121558));
#8281=CARTESIAN_POINT('',(-4.9614889151716,-6.5,79.5607698662059));
#8282=CARTESIAN_POINT('',(-5.04763303690956,-6.5,79.8655396305548));
#8283=CARTESIAN_POINT('',(-4.9614889151716,-4.5,79.5607698662059));
#8284=CARTESIAN_POINT('Origin',(-4.86876234485807,-4.5,79.6033865015699));
#8285=CARTESIAN_POINT('',(-4.86876234485807,-2.5,79.6033865015699));
#8286=CARTESIAN_POINT('',(-8.73404532801766,-2.5,77.8269231328196));
#8287=CARTESIAN_POINT('',(-4.86876234485807,-6.5,79.6033865015699));
#8288=CARTESIAN_POINT('',(-5.61320904050309,-6.5,79.2612427851687));
#8289=CARTESIAN_POINT('',(-4.86876234485807,-4.5,79.6033865015699));
#8290=CARTESIAN_POINT('Origin',(-0.981142563718946,-4.5,73.9056856751205));
#8291=CARTESIAN_POINT('',(5.05696247920323,-2.5,65.0562307309528));
#8292=CARTESIAN_POINT('',(-5.04763303690956,-6.5,79.8655396305548));
#8293=CARTESIAN_POINT('Origin',(-17.1105963211311,-4.5,74.8692033194898));
#8294=CARTESIAN_POINT('',(-17.1105963211311,-2.5,74.8692033194898));
#8295=CARTESIAN_POINT('',(-7.15787945733663,-2.5,62.9164184678592));
#8296=CARTESIAN_POINT('',(-17.1105963211311,-6.5,74.8692033194898));
#8297=CARTESIAN_POINT('',(-17.3132539231097,-6.5,75.1125863824411));
#8298=CARTESIAN_POINT('',(-17.1105963211311,-4.5,74.8692033194898));
#8299=CARTESIAN_POINT('Origin',(-17.0432201312256,-4.5,74.9458508470798));
#8300=CARTESIAN_POINT('',(-17.0432201312256,-2.5,74.9458508470798));
#8301=CARTESIAN_POINT('',(-19.8517790958416,-2.5,71.7508185807811));
#8302=CARTESIAN_POINT('',(-17.0432201312256,-6.5,74.9458508470798));
#8303=CARTESIAN_POINT('',(-17.5841436418306,-6.5,74.330493259165));
#8304=CARTESIAN_POINT('',(-17.0432201312256,-4.5,74.9458508470798));
#8305=CARTESIAN_POINT('Origin',(-11.1742390317242,-4.5,71.3219795574061));
#8306=CARTESIAN_POINT('',(-2.05875799995239,-2.5,65.693518766246));
#8307=CARTESIAN_POINT('',(-17.3132539231097,-6.5,75.1125863824411));
#8308=CARTESIAN_POINT('Origin',(-30.9439523809731,-4.5,53.4739397777569));
#8309=CARTESIAN_POINT('',(-30.9439523809731,-2.5,53.4739397777569));
#8310=CARTESIAN_POINT('',(-15.4016346984504,-2.5,52.8722756390788));
#8311=CARTESIAN_POINT('',(-30.9439523809731,-6.5,53.4739397777569));
#8312=CARTESIAN_POINT('',(-31.2604256489094,-6.5,53.4861908859929));
#8313=CARTESIAN_POINT('',(-30.9439523809731,-4.5,53.4739397777569));
#8314=CARTESIAN_POINT('Origin',(-30.9558291236816,-4.5,53.5752972512578));
#8315=CARTESIAN_POINT('',(-30.9558291236816,-2.5,53.5752972512578));
#8316=CARTESIAN_POINT('',(-30.4607501907366,-2.5,49.3502373119707));
#8317=CARTESIAN_POINT('',(-30.9558291236816,-6.5,53.5752972512578));
#8318=CARTESIAN_POINT('',(-30.8604777930494,-6.5,52.7615581474436));
#8319=CARTESIAN_POINT('',(-30.9558291236816,-4.5,53.5752972512578));
#8320=CARTESIAN_POINT('Origin',(-24.3356530447464,-4.5,55.5119569927511));
#8321=CARTESIAN_POINT('',(-14.0534441823513,-2.5,58.5199041711936));
#8322=CARTESIAN_POINT('',(-31.2604256489094,-6.5,53.4861908859929));
#8323=CARTESIAN_POINT('Origin',(7.67452462700238,-4.5,47.8864583401654));
#8324=CARTESIAN_POINT('',(3.83726231350119,-2.5,47.8864583401654));
#8325=CARTESIAN_POINT('',(21.2750522452644,-6.5,47.8864583401654));
#8326=CARTESIAN_POINT('Origin',(21.2750522452644,-4.5,49.3864583401654));
#8327=CARTESIAN_POINT('',(10.6375261226322,-2.5,49.3864583401654));
#8328=CARTESIAN_POINT('',(7.67452462700238,-6.5,49.3864583401654));
#8329=CARTESIAN_POINT('Origin',(0.,-4.5,48.6364583401654));
#8330=CARTESIAN_POINT('',(-1.99137169252308,-2.5,48.6364583401654));
#8331=CARTESIAN_POINT('Origin',(0.,-2.5,48.6364583401654));
#8332=CARTESIAN_POINT('',(-1.99137169252308,-6.5,48.6364583401654));
#8333=CARTESIAN_POINT('',(-1.99137169252308,-4.5,48.6364583401654));
#8334=CARTESIAN_POINT('Origin',(0.,-6.5,48.6364583401654));
#8335=CARTESIAN_POINT('Origin',(0.,-2.5,48.6364583401654));
#8336=CARTESIAN_POINT('Origin',(0.,-6.5,48.6364583401654));
#8337=CARTESIAN_POINT('',(0.,0.,0.));
#8338=CARTESIAN_POINT('Origin',(0.,2.,92.461739559435));
#8339=CARTESIAN_POINT('',(-1.26938918348039,4.,92.461739559435));
#8340=CARTESIAN_POINT('Origin',(0.,4.,92.461739559435));
#8341=CARTESIAN_POINT('',(-1.26938918348039,2.,92.461739559435));
#8342=CARTESIAN_POINT('',(-1.26938918348039,2.,92.461739559435));
#8343=CARTESIAN_POINT('Origin',(0.,2.,92.461739559435));
#8344=CARTESIAN_POINT('Origin',(-2.,2.,95.8170335569158));
#8345=CARTESIAN_POINT('',(-2.,2.,0.));
#8346=CARTESIAN_POINT('',(-2.,2.,95.8170335569158));
#8347=CARTESIAN_POINT('',(-2.,2.,0.));
#8348=CARTESIAN_POINT('',(-2.,4.,95.8170335569158));
#8349=CARTESIAN_POINT('',(-2.,2.,95.8170335569158));
#8350=CARTESIAN_POINT('',(-2.,4.,0.));
#8351=CARTESIAN_POINT('',(-2.,4.,0.));
#8352=CARTESIAN_POINT('',(-2.,2.,0.));
#8353=CARTESIAN_POINT('Origin',(2.,2.,0.));
#8354=CARTESIAN_POINT('',(2.,2.,0.));
#8355=CARTESIAN_POINT('',(0.,2.,0.));
#8356=CARTESIAN_POINT('',(2.,4.,0.));
#8357=CARTESIAN_POINT('',(0.,4.,0.));
#8358=CARTESIAN_POINT('',(2.,2.,0.));
#8359=CARTESIAN_POINT('Origin',(2.,2.,95.8170335569158));
#8360=CARTESIAN_POINT('',(2.,2.,95.8170335569158));
#8361=CARTESIAN_POINT('',(2.,2.,0.));
#8362=CARTESIAN_POINT('',(2.,4.,95.8170335569158));
#8363=CARTESIAN_POINT('',(2.,4.,0.));
#8364=CARTESIAN_POINT('',(2.,2.,95.8170335569158));
#8365=CARTESIAN_POINT('Origin',(0.,2.,95.8170335569158));
#8366=CARTESIAN_POINT('',(2.,2.,95.8170335569158));
#8367=CARTESIAN_POINT('',(-2.,4.,95.8170335569158));
#8368=CARTESIAN_POINT('Origin',(1.,4.,47.9085167784579));
#8369=CARTESIAN_POINT('Origin',(1.,2.,47.9085167784579));
#8370=CARTESIAN_POINT('',(0.,0.,0.));
#8371=CARTESIAN_POINT('Origin',(22.0759476067182,-6.5,76.7431289545307));
#8372=CARTESIAN_POINT('',(4.09006724262322,-6.5,87.3069627514587));
#8373=CARTESIAN_POINT('',(22.0759476067182,-6.5,76.7431289545307));
#8374=CARTESIAN_POINT('',(4.09006724262322,-6.5,87.3069627514587));
#8375=CARTESIAN_POINT('',(4.09006724262321,-2.5,87.3069627514587));
#8376=CARTESIAN_POINT('',(4.09006724262322,-6.5,87.3069627514587));
#8377=CARTESIAN_POINT('',(22.0759476067182,-2.5,76.7431289545307));
#8378=CARTESIAN_POINT('',(11.5910700858341,-2.5,82.9013208956311));
#8379=CARTESIAN_POINT('',(22.0759476067182,-4.5,76.7431289545307));
#8380=CARTESIAN_POINT('Origin',(-4.29634599084193,-6.5,87.477586159287));
#8381=CARTESIAN_POINT('',(-4.29634599084193,-6.5,87.477586159287));
#8382=CARTESIAN_POINT('',(-24.0531806351797,-6.5,75.634931048273));
#8383=CARTESIAN_POINT('',(-4.29634599084193,-6.5,87.477586159287));
#8384=CARTESIAN_POINT('',(-24.0531806351797,-2.5,75.634931048273));
#8385=CARTESIAN_POINT('',(-24.0531806351797,-4.5,75.634931048273));
#8386=CARTESIAN_POINT('',(-4.29634599084193,-2.5,87.477586159287));
#8387=CARTESIAN_POINT('',(-3.96187942842657,-2.5,87.6780723310932));
#8388=CARTESIAN_POINT('',(-4.29634599084193,-6.5,87.477586159287));
#8389=CARTESIAN_POINT('Origin',(0.,-6.5,92.461739559435));
#8390=CARTESIAN_POINT('Origin',(0.,-6.5,92.461739559435));
#8391=CARTESIAN_POINT('Origin',(0.,-2.5,92.461739559435));
#8392=CARTESIAN_POINT('Origin',(0.,-6.5,102.055558916393));
#8393=CARTESIAN_POINT('',(0.,-6.5,102.055558916393));
#8394=CARTESIAN_POINT('',(28.7457294952528,-6.5,74.4504008586727));
#8395=CARTESIAN_POINT('',(0.,-6.5,102.055558916393));
#8396=CARTESIAN_POINT('',(28.7457294952528,-2.5,74.4504008586727));
#8397=CARTESIAN_POINT('',(28.7457294952528,-4.5,74.4504008586727));
#8398=CARTESIAN_POINT('',(0.,-2.5,102.055558916393));
#8399=CARTESIAN_POINT('',(3.97893495048528,-2.5,98.234499922998));
#8400=CARTESIAN_POINT('',(0.,-6.5,102.055558916393));
#8401=CARTESIAN_POINT('Origin',(-31.9194481137532,-6.5,72.0694672890556));
#8402=CARTESIAN_POINT('',(-31.9194481137532,-6.5,72.0694672890556));
#8403=CARTESIAN_POINT('',(0.,-6.5,102.055558916393));
#8404=CARTESIAN_POINT('',(-31.9194481137532,-2.5,72.0694672890556));
#8405=CARTESIAN_POINT('',(-20.7679309766169,-2.5,82.545538600386));
#8406=CARTESIAN_POINT('',(-31.9194481137532,-4.5,72.0694672890556));
#8407=CARTESIAN_POINT('Origin',(0.,-4.5,92.461739559435));
#8408=CARTESIAN_POINT('',(-1.26938918348039,-2.5,92.461739559435));
#8409=CARTESIAN_POINT('Origin',(0.,-2.5,92.461739559435));
#8410=CARTESIAN_POINT('',(-1.26938918348039,-6.5,92.461739559435));
#8411=CARTESIAN_POINT('',(-1.26938918348039,-4.5,92.461739559435));
#8412=CARTESIAN_POINT('Origin',(0.,-6.5,92.461739559435));
#8413=CARTESIAN_POINT('Origin',(22.9001701836232,-4.5,68.948697977139));
#8414=CARTESIAN_POINT('',(22.9001701836232,-2.5,68.948697977139));
#8415=CARTESIAN_POINT('',(20.2820284879064,-2.5,66.4845646164644));
#8416=CARTESIAN_POINT('',(22.9001701836232,-6.5,68.948697977139));
#8417=CARTESIAN_POINT('',(28.7457294952528,-6.5,74.4504008586727));
#8418=CARTESIAN_POINT('',(22.9001701836232,-4.5,68.948697977139));
#8419=CARTESIAN_POINT('Origin',(35.4950562068848,-4.5,74.2213391862183));
#8420=CARTESIAN_POINT('Origin',(35.4950562068848,-2.5,74.2213391862183));
#8421=CARTESIAN_POINT('Origin',(35.4950562068848,-6.5,74.2213391862183));
#8422=CARTESIAN_POINT('Origin',(-20.4586462226688,-4.5,71.5270410964181));
#8423=CARTESIAN_POINT('',(-20.4586462226688,-2.5,71.5270410964181));
#8424=CARTESIAN_POINT('',(-19.5750050436382,-2.5,70.5172021843879));
#8425=CARTESIAN_POINT('',(-20.4586462226688,-6.5,71.5270410964181));
#8426=CARTESIAN_POINT('',(-20.4586462226688,-6.5,71.5270410964181));
#8427=CARTESIAN_POINT('',(-20.4586462226688,-4.5,71.5270410964181));
#8428=CARTESIAN_POINT('Origin',(-25.4984288865264,-4.5,86.3901736394385));
#8429=CARTESIAN_POINT('Origin',(-25.4984288865264,-2.5,86.3901736394385));
#8430=CARTESIAN_POINT('Origin',(-25.4984288865264,-6.5,86.3901736394385));
#8431=CARTESIAN_POINT('Origin',(-1.5868593092502,-2.5,84.4743489885695));
#8432=CARTESIAN_POINT('Origin',(-1.5868593092502,-6.5,84.4743489885695));
#8433=CARTESIAN_POINT('',(0.,0.,0.));
#8434=CARTESIAN_POINT('Origin',(0.,0.,92.461739559435));
#8435=CARTESIAN_POINT('',(-2.00038918348039,4.,92.461739559435));
#8436=CARTESIAN_POINT('Origin',(0.,4.,92.461739559435));
#8437=CARTESIAN_POINT('',(-2.00038918348039,-6.,92.461739559435));
#8438=CARTESIAN_POINT('',(-2.00038918348039,0.,92.461739559435));
#8439=CARTESIAN_POINT('Origin',(0.,-6.,92.461739559435));
#8440=CARTESIAN_POINT('Origin',(0.,-6.,92.461739559435));
#8441=CARTESIAN_POINT('Origin',(1.,4.,47.9085167784579));
#8442=CARTESIAN_POINT('',(0.,0.,0.));
#8443=CARTESIAN_POINT('Origin',(0.,-6.5,48.6364583401654));
#8444=CARTESIAN_POINT('',(3.,-6.5,48.6364583401654));
#8445=CARTESIAN_POINT('Origin',(0.,-6.5,48.6364583401654));
#8446=CARTESIAN_POINT('',(-1.99137169252308,-6.5,48.6364583401654));
#8447=CARTESIAN_POINT('Origin',(0.,-6.5,48.6364583401654));
#8448=CARTESIAN_POINT('Origin',(0.,-8.30780358767644,48.1364583401654));
#8449=CARTESIAN_POINT('',(2.90166314701339,-6.69219641232357,48.1364583401654));
#8450=CARTESIAN_POINT('',(1.70338802732979,-7.5,48.1364583401654));
#8451=CARTESIAN_POINT('Ctrl Pts',(2.90166314701339,-6.69219641232357,48.1364583401654));
#8452=CARTESIAN_POINT('Ctrl Pts',(2.89738588729895,-6.70334128000014,48.1364583401654));
#8453=CARTESIAN_POINT('Ctrl Pts',(2.89299471233252,-6.7143000212193,48.1364583401654));
#8454=CARTESIAN_POINT('Ctrl Pts',(2.8291108799372,-6.86750715654011,48.1364583401654));
#8455=CARTESIAN_POINT('Ctrl Pts',(2.72552921913,-7.02105058333943,48.1364583401654));
#8456=CARTESIAN_POINT('Ctrl Pts',(2.50478431602599,-7.23991674541786,48.1364583401654));
#8457=CARTESIAN_POINT('Ctrl Pts',(2.34795167915788,-7.34324272062795,48.1364583401654));
#8458=CARTESIAN_POINT('Ctrl Pts',(2.05411736736806,-7.46354654155341,48.1364583401654));
#8459=CARTESIAN_POINT('Ctrl Pts',(1.86438783412795,-7.5,48.1364583401654));
#8460=CARTESIAN_POINT('Ctrl Pts',(1.70338802732979,-7.5,48.1364583401654));
#8461=CARTESIAN_POINT('',(-2.90166314701339,-6.69219641232357,48.1364583401654));
#8462=CARTESIAN_POINT('',(0.,-6.69219641232357,48.1364583401654));
#8463=CARTESIAN_POINT('',(-1.70338802732979,-7.5,48.1364583401654));
#8464=CARTESIAN_POINT('Ctrl Pts',(-1.70338802732979,-7.5,48.1364583401654));
#8465=CARTESIAN_POINT('Ctrl Pts',(-1.86438783412795,-7.5,48.1364583401654));
#8466=CARTESIAN_POINT('Ctrl Pts',(-2.05411736736806,-7.46354654155341,48.1364583401654));
#8467=CARTESIAN_POINT('Ctrl Pts',(-2.34795167915788,-7.34324272062795,48.1364583401654));
#8468=CARTESIAN_POINT('Ctrl Pts',(-2.50478431602599,-7.23991674541786,48.1364583401654));
#8469=CARTESIAN_POINT('Ctrl Pts',(-2.72552921913,-7.02105058333943,48.1364583401654));
#8470=CARTESIAN_POINT('Ctrl Pts',(-2.8291108799372,-6.86750715654011,48.1364583401654));
#8471=CARTESIAN_POINT('Ctrl Pts',(-2.89299471233252,-6.7143000212193,48.1364583401654));
#8472=CARTESIAN_POINT('Ctrl Pts',(-2.89738588729895,-6.70334128000014,48.1364583401654));
#8473=CARTESIAN_POINT('Ctrl Pts',(-2.90166314701339,-6.69219641232357,48.1364583401654));
#8474=CARTESIAN_POINT('',(0.,-7.5,48.1364583401654));
#8475=CARTESIAN_POINT('Origin',(0.,-6.69219641232357,48.1364583401654));
#8476=CARTESIAN_POINT('',(2.90166314701339,-6.69219641232357,49.1364583401654));
#8477=CARTESIAN_POINT('',(2.94442677252053,-6.69219641232357,48.6364583401654));
#8478=CARTESIAN_POINT('Origin',(0.,-6.69219641232357,48.6364583401654));
#8479=CARTESIAN_POINT('',(-2.90166314701339,-6.69219641232357,49.1364583401654));
#8480=CARTESIAN_POINT('',(0.,-6.69219641232357,49.1364583401654));
#8481=CARTESIAN_POINT('Origin',(0.,-6.69219641232357,48.6364583401654));
#8482=CARTESIAN_POINT('Origin',(0.,-6.69219641232357,48.6364583401654));
#8483=CARTESIAN_POINT('Origin',(0.,-6.69219641232357,49.1364583401654));
#8484=CARTESIAN_POINT('',(1.70338802732979,-7.5,49.1364583401654));
#8485=CARTESIAN_POINT('Ctrl Pts',(1.70338802732979,-7.5,49.1364583401654));
#8486=CARTESIAN_POINT('Ctrl Pts',(1.86438783412795,-7.5,49.1364583401654));
#8487=CARTESIAN_POINT('Ctrl Pts',(2.05411736736806,-7.46354654155341,49.1364583401654));
#8488=CARTESIAN_POINT('Ctrl Pts',(2.34795167915788,-7.34324272062795,49.1364583401654));
#8489=CARTESIAN_POINT('Ctrl Pts',(2.50478431602599,-7.23991674541786,49.1364583401654));
#8490=CARTESIAN_POINT('Ctrl Pts',(2.72552921913,-7.02105058333943,49.1364583401654));
#8491=CARTESIAN_POINT('Ctrl Pts',(2.8291108799372,-6.86750715654011,49.1364583401654));
#8492=CARTESIAN_POINT('Ctrl Pts',(2.89299471233252,-6.7143000212193,49.1364583401654));
#8493=CARTESIAN_POINT('Ctrl Pts',(2.89738588729895,-6.70334128000014,49.1364583401654));
#8494=CARTESIAN_POINT('Ctrl Pts',(2.90166314701339,-6.69219641232357,49.1364583401654));
#8495=CARTESIAN_POINT('',(-1.70338802732979,-7.5,49.1364583401654));
#8496=CARTESIAN_POINT('',(0.,-7.5,49.1364583401654));
#8497=CARTESIAN_POINT('Ctrl Pts',(-2.90166314701339,-6.69219641232357,49.1364583401654));
#8498=CARTESIAN_POINT('Ctrl Pts',(-2.89738588729895,-6.70334128000014,49.1364583401654));
#8499=CARTESIAN_POINT('Ctrl Pts',(-2.89299471233252,-6.7143000212193,49.1364583401654));
#8500=CARTESIAN_POINT('Ctrl Pts',(-2.8291108799372,-6.86750715654011,49.1364583401654));
#8501=CARTESIAN_POINT('Ctrl Pts',(-2.72552921913,-7.02105058333943,49.1364583401654));
#8502=CARTESIAN_POINT('Ctrl Pts',(-2.50478431602599,-7.23991674541786,49.1364583401654));
#8503=CARTESIAN_POINT('Ctrl Pts',(-2.34795167915788,-7.34324272062795,49.1364583401654));
#8504=CARTESIAN_POINT('Ctrl Pts',(-2.05411736736806,-7.46354654155341,49.1364583401654));
#8505=CARTESIAN_POINT('Ctrl Pts',(-1.86438783412795,-7.5,49.1364583401654));
#8506=CARTESIAN_POINT('Ctrl Pts',(-1.70338802732979,-7.5,49.1364583401654));
#8507=CARTESIAN_POINT('Origin',(0.,-7.5,48.6364583401654));
#8508=CARTESIAN_POINT('Origin',(0.,-7.5,48.6364583401654));
#8509=CARTESIAN_POINT('Origin',(0.,-6.25,48.6364583401654));
#8510=CARTESIAN_POINT('Origin',(1.77525512860841,-6.25,48.6364583401654));
#8511=CARTESIAN_POINT('Origin',(0.,-7.5,48.6364583401654));
#8512=CARTESIAN_POINT('Origin',(0.,-7.5,48.6364583401654));
#8513=CARTESIAN_POINT('Origin',(0.,-2.5,48.6364583401654));
#8514=CARTESIAN_POINT('',(-1.99137169252308,-2.5,48.6364583401654));
#8515=CARTESIAN_POINT('Origin',(0.,-2.5,48.6364583401654));
#8516=CARTESIAN_POINT('Origin',(0.,-6.,48.6364583401654));
#8517=CARTESIAN_POINT('',(-1.99137169252308,-6.,48.6364583401654));
#8518=CARTESIAN_POINT('',(0.,0.,0.));
#8519=CARTESIAN_POINT('Origin',(0.,2.,48.6364583401654));
#8520=CARTESIAN_POINT('',(-1.99137169252308,-6.,48.6364583401654));
#8521=CARTESIAN_POINT('Origin',(0.,-6.,48.6364583401654));
#8522=CARTESIAN_POINT('',(-1.99137169252308,2.,48.6364583401654));
#8523=CARTESIAN_POINT('',(-1.99137169252308,2.,48.6364583401654));
#8524=CARTESIAN_POINT('Origin',(0.,2.,48.6364583401654));
#8525=CARTESIAN_POINT('Origin',(0.,-6.,48.6364583401654));
#8526=CARTESIAN_POINT('Origin',(0.,2.,48.6364583401654));
#8527=CARTESIAN_POINT('',(0.,0.,0.));
#8528=CARTESIAN_POINT('Origin',(-1.8,0.,0.));
#8529=CARTESIAN_POINT('',(-1.7,4.8,-5.8783046359073E-16));
#8530=CARTESIAN_POINT('Origin',(-1.7,1.83697019872105E-17,0.));
#8531=CARTESIAN_POINT('',(-1.955,4.8,-5.8783046359073E-16));
#8532=CARTESIAN_POINT('',(-1.8,4.8,-5.87830463590729E-16));
#8533=CARTESIAN_POINT('Origin',(-1.955,-2.84730380801758E-17,0.));
#8534=CARTESIAN_POINT('Origin',(-1.8,0.,0.));
#8535=CARTESIAN_POINT('',(1.7,4.872,-5.96647920544591E-16));
#8536=CARTESIAN_POINT('Origin',(1.7,6.42939569552361E-16,0.));
#8537=CARTESIAN_POINT('',(-1.7,4.872,-5.96647920544591E-16));
#8538=CARTESIAN_POINT('',(-1.8,4.872,-5.96647920544591E-16));
#8539=CARTESIAN_POINT('Origin',(-1.7,1.83697019872105E-17,0.));
#8540=CARTESIAN_POINT('Origin',(-1.8,0.,0.));
#8541=CARTESIAN_POINT('',(1.955,-4.8,5.90585918888811E-16));
#8542=CARTESIAN_POINT('',(1.955,4.8,-5.87830463590729E-16));
#8543=CARTESIAN_POINT('Origin',(1.955,6.89782309619747E-16,0.));
#8544=CARTESIAN_POINT('Origin',(1.955,6.89782309619747E-16,0.));
#8545=CARTESIAN_POINT('',(1.7,4.8,-5.87830463590729E-16));
#8546=CARTESIAN_POINT('',(-1.8,4.8,-5.87830463590729E-16));
#8547=CARTESIAN_POINT('Origin',(1.7,6.42939569552361E-16,0.));
#8548=CARTESIAN_POINT('Origin',(1.955,6.89782309619747E-16,0.));
#8549=CARTESIAN_POINT('',(2.,-4.845,-5.93341374186893E-16));
#8550=CARTESIAN_POINT('',(1.955,-4.8,-5.87830463590729E-16));
#8551=CARTESIAN_POINT('Origin',(2.,6.98048675513991E-16,0.));
#8552=CARTESIAN_POINT('Origin',(1.8,8.67361737988404E-16,0.));
#8553=CARTESIAN_POINT('',(1.8,6.,-7.34788079488412E-16));
#8554=CARTESIAN_POINT('Origin',(1.8,6.61309271539571E-16,0.));
#8555=CARTESIAN_POINT('',(2.,5.8,-7.10295143505465E-16));
#8556=CARTESIAN_POINT('Origin',(1.8,5.8,-7.10295143505465E-16));
#8557=CARTESIAN_POINT('Origin',(2.,6.98048675513991E-16,0.));
#8558=CARTESIAN_POINT('Origin',(-1.8,0.,0.));
#8559=CARTESIAN_POINT('',(-1.8,6.,-7.34788079488412E-16));
#8560=CARTESIAN_POINT('Origin',(-1.8,2.02467570659351E-31,0.));
#8561=CARTESIAN_POINT('',(-1.8,6.,-7.34788079488412E-16));
#8562=CARTESIAN_POINT('Origin',(-1.8,0.,0.));
#8563=CARTESIAN_POINT('',(-2.,5.8,-7.10295143505465E-16));
#8564=CARTESIAN_POINT('Origin',(-2.,-3.67394039744204E-17,0.));
#8565=CARTESIAN_POINT('Origin',(-1.8,5.8,-7.10295143505465E-16));
#8566=CARTESIAN_POINT('Origin',(-2.,-3.67394039744204E-17,0.));
#8567=CARTESIAN_POINT('',(-2.,4.845,-5.93341374186893E-16));
#8568=CARTESIAN_POINT('',(-2.,4.845,-5.93341374186893E-16));
#8569=CARTESIAN_POINT('Origin',(-2.,-3.67394039744204E-17,0.));
#8570=CARTESIAN_POINT('Origin',(-2.,5.8,0.));
#8571=CARTESIAN_POINT('Origin',(2.,5.8,0.));
#8572=CARTESIAN_POINT('Origin',(1.7,4.8,0.));
#8573=CARTESIAN_POINT('Origin',(-1.7,4.8,0.));
#8574=CARTESIAN_POINT('Origin',(-1.955,-2.84730380801757E-17,0.));
#8575=CARTESIAN_POINT('',(-1.955,3.1184375,3.81898450271607E-16));
#8576=CARTESIAN_POINT('',(-1.955,-3.1184375,-3.81898450271607E-16));
#8577=CARTESIAN_POINT('Origin',(-1.955,-2.84730380801757E-17,0.));
#8578=CARTESIAN_POINT('',(-2.,-3.0734375,-3.76387539675444E-16));
#8579=CARTESIAN_POINT('',(-1.955,-3.1184375,-3.81898450271607E-16));
#8580=CARTESIAN_POINT('Origin',(-2.,-3.67394039744204E-17,0.));
#8581=CARTESIAN_POINT('Origin',(-1.955,-2.84730380801757E-17,0.));
#8582=CARTESIAN_POINT('Origin',(-1.8,0.,0.));
#8583=CARTESIAN_POINT('',(-1.7890625,3.1184375,-3.81898450271607E-16));
#8584=CARTESIAN_POINT('',(-1.8,3.1184375,-3.81898450271607E-16));
#8585=CARTESIAN_POINT('Origin',(-1.7890625,2.00918615485137E-18,0.));
#8586=CARTESIAN_POINT('Origin',(-1.7890625,0.,0.));
#8587=CARTESIAN_POINT('',(-1.6625,3.2,-3.91886975727153E-16));
#8588=CARTESIAN_POINT('Origin',(-1.7890625,3.25741379310345,-3.98918137522258E-16));
#8589=CARTESIAN_POINT('Origin',(-1.6625,2.52583402324144E-17,0.));
#8590=CARTESIAN_POINT('Origin',(-1.8,0.,0.));
#8591=CARTESIAN_POINT('',(-1.6625,3.272,-4.00704432681014E-16));
#8592=CARTESIAN_POINT('Origin',(-1.6625,2.52583402324144E-17,0.));
#8593=CARTESIAN_POINT('',(1.6625,3.272,-4.00704432681014E-16));
#8594=CARTESIAN_POINT('',(-1.8,3.272,-4.00704432681014E-16));
#8595=CARTESIAN_POINT('Origin',(1.6625,6.36050931307157E-16,0.));
#8596=CARTESIAN_POINT('Origin',(1.7890625,8.67361737988404E-16,0.));
#8597=CARTESIAN_POINT('',(1.6625,3.2,-3.91886975727153E-16));
#8598=CARTESIAN_POINT('Origin',(1.6625,6.36050931307157E-16,0.));
#8599=CARTESIAN_POINT('',(1.7890625,3.1184375,-3.81898450271607E-16));
#8600=CARTESIAN_POINT('Origin',(1.7890625,3.25741379310345,-3.98918137522258E-16));
#8601=CARTESIAN_POINT('Origin',(1.7890625,6.5930008538472E-16,0.));
#8602=CARTESIAN_POINT('Origin',(-1.8,0.,0.));
#8603=CARTESIAN_POINT('',(1.955,3.1184375,-3.81898450271607E-16));
#8604=CARTESIAN_POINT('',(-1.8,3.1184375,-3.81898450271607E-16));
#8605=CARTESIAN_POINT('Origin',(1.955,6.89782309619747E-16,0.));
#8606=CARTESIAN_POINT('Origin',(2.,6.98048675513991E-16,0.));
#8607=CARTESIAN_POINT('',(2.,3.0734375,-3.76387539675444E-16));
#8608=CARTESIAN_POINT('',(2.,3.0734375,-3.76387539675444E-16));
#8609=CARTESIAN_POINT('Origin',(2.,6.98048675513991E-16,0.));
#8610=CARTESIAN_POINT('Origin',(1.8,8.67361737988404E-16,0.));
#8611=CARTESIAN_POINT('',(2.,2.2,-2.69422295812418E-16));
#8612=CARTESIAN_POINT('Origin',(2.,6.98048675513991E-16,0.));
#8613=CARTESIAN_POINT('',(1.8,2.,-2.44929359829471E-16));
#8614=CARTESIAN_POINT('Origin',(1.8,2.2,-2.69422295812418E-16));
#8615=CARTESIAN_POINT('Origin',(1.8,6.61309271539571E-16,0.));
#8616=CARTESIAN_POINT('Origin',(-1.8,0.,0.));
#8617=CARTESIAN_POINT('',(-1.8,2.,-2.44929359829471E-16));
#8618=CARTESIAN_POINT('',(-1.8,2.,-2.44929359829471E-16));
#8619=CARTESIAN_POINT('Origin',(-1.8,1.86988015034452E-31,0.));
#8620=CARTESIAN_POINT('Origin',(-1.8,0.,0.));
#8621=CARTESIAN_POINT('',(-2.,2.2,-2.69422295812418E-16));
#8622=CARTESIAN_POINT('Origin',(-1.8,2.2,-2.69422295812418E-16));
#8623=CARTESIAN_POINT('Origin',(-2.,-3.67394039744205E-17,0.));
#8624=CARTESIAN_POINT('Origin',(2.,2.2,0.));
#8625=CARTESIAN_POINT('Origin',(1.6625,3.272,0.));
#8626=CARTESIAN_POINT('Origin',(-1.6625,3.2,0.));
#8627=CARTESIAN_POINT('Origin',(-2.,2.2,0.));
#8628=CARTESIAN_POINT('Origin',(-1.8,0.,0.));
#8629=CARTESIAN_POINT('',(1.95,3.2,-3.91886975727153E-16));
#8630=CARTESIAN_POINT('Origin',(1.95,6.88863824520387E-16,0.));
#8631=CARTESIAN_POINT('',(1.85,3.2,-3.91886975727153E-16));
#8632=CARTESIAN_POINT('',(-1.8,3.2,-3.91886975727153E-16));
#8633=CARTESIAN_POINT('Origin',(1.85,6.70494122533176E-16,0.));
#8634=CARTESIAN_POINT('Origin',(1.86,8.67361737988404E-16,0.));
#8635=CARTESIAN_POINT('',(1.905,4.22108058265378,-5.16933282449E-16));
#8636=CARTESIAN_POINT('Origin',(1.905,6.80597458626142E-16,0.));
#8637=CARTESIAN_POINT('',(1.95,4.14313829631318,-5.07388105300476E-16));
#8638=CARTESIAN_POINT('Origin',(1.86,4.14313829631318,-5.07388105300475E-16));
#8639=CARTESIAN_POINT('Origin',(1.95,6.88863824520387E-16,0.));
#8640=CARTESIAN_POINT('Origin',(1.65333333333334,6.34367041958329E-16,0.));
#8641=CARTESIAN_POINT('',(1.65333333333334,4.36638040039984,-5.3472737812094E-16));
#8642=CARTESIAN_POINT('Origin',(1.65333333333334,6.34367041958329E-16,0.));
#8643=CARTESIAN_POINT('',(1.65333333333334,4.36638040039984,-5.3472737812094E-16));
#8644=CARTESIAN_POINT('Origin',(1.66333333333334,8.67361737988404E-16,0.));
#8645=CARTESIAN_POINT('',(1.64333333333333,4.38370090847553,-5.3684852859839E-16));
#8646=CARTESIAN_POINT('Origin',(1.64333333333334,6.32530071759608E-16,0.));
#8647=CARTESIAN_POINT('Origin',(1.66333333333334,4.38370090847553,-5.3684852859839E-16));
#8648=CARTESIAN_POINT('Origin',(1.76333333333333,8.67361737988404E-16,0.));
#8649=CARTESIAN_POINT('',(1.86725638178747,4.64,-5.68236114804372E-16));
#8650=CARTESIAN_POINT('Origin',(1.86725638178747,6.73664068441309E-16,0.));
#8651=CARTESIAN_POINT('',(1.64333333333333,4.58,-5.60888234009488E-16));
#8652=CARTESIAN_POINT('Origin',(1.76333333333333,4.58,-5.60888234009488E-16));
#8653=CARTESIAN_POINT('Origin',(1.64333333333334,6.32530071759608E-16,0.));
#8654=CARTESIAN_POINT('Origin',(1.90725638178747,6.81011949236193E-16,0.));
#8655=CARTESIAN_POINT('',(1.90725638178747,4.57071796769724,-5.59751512894572E-16));
#8656=CARTESIAN_POINT('Origin',(1.90725638178747,6.81011949236193E-16,0.));
#8657=CARTESIAN_POINT('',(1.90725638178747,4.57071796769724,-5.59751512894572E-16));
#8658=CARTESIAN_POINT('Origin',(1.80333333333334,8.67361737988404E-16,0.));
#8659=CARTESIAN_POINT('',(1.80333333333334,4.39071796769724,-5.3770787050992E-16));
#8660=CARTESIAN_POINT('Origin',(1.80333333333334,6.61921594939145E-16,0.));
#8661=CARTESIAN_POINT('Origin',(1.80333333333334,4.51071796769724,-5.52403632099688E-16));
#8662=CARTESIAN_POINT('Origin',(1.80333333333334,8.67361737988404E-16,0.));
#8663=CARTESIAN_POINT('',(1.99385892216591,4.62071796769724,-5.65874746890309E-16));
#8664=CARTESIAN_POINT('Origin',(1.99385892216591,6.96920577817067E-16,0.));
#8665=CARTESIAN_POINT('',(1.80333333333334,4.29071796769724,-5.25461402518447E-16));
#8666=CARTESIAN_POINT('Origin',(1.80333333333334,4.51071796769724,-5.52403632099688E-16));
#8667=CARTESIAN_POINT('Origin',(1.80333333333334,6.61921594939145E-16,0.));
#8668=CARTESIAN_POINT('Origin',(1.99385892216591,6.96920577817067E-16,0.));
#8669=CARTESIAN_POINT('',(1.95385892216591,4.69,-5.74359348800109E-16));
#8670=CARTESIAN_POINT('Origin',(1.95385892216591,6.89572697022182E-16,0.));
#8671=CARTESIAN_POINT('',(1.99385892216591,4.62071796769724,-5.65874746890309E-16));
#8672=CARTESIAN_POINT('Origin',(1.76333333333333,8.67361737988404E-16,0.));
#8673=CARTESIAN_POINT('',(1.54333333333334,4.58,-5.60888234009488E-16));
#8674=CARTESIAN_POINT('Origin',(1.54333333333334,6.14160369772398E-16,0.));
#8675=CARTESIAN_POINT('Origin',(1.76333333333333,4.58,-5.60888234009488E-16));
#8676=CARTESIAN_POINT('Origin',(1.66333333333334,8.67361737988404E-16,0.));
#8677=CARTESIAN_POINT('',(1.60333333333334,4.27977786002139,-5.24121625733691E-16));
#8678=CARTESIAN_POINT('Origin',(1.60333333333334,6.25182190964724E-16,0.));
#8679=CARTESIAN_POINT('',(1.54333333333333,4.38370090847553,-5.3684852859839E-16));
#8680=CARTESIAN_POINT('Origin',(1.66333333333334,4.38370090847553,-5.3684852859839E-16));
#8681=CARTESIAN_POINT('Origin',(1.54333333333334,6.14160369772398E-16,0.));
#8682=CARTESIAN_POINT('Origin',(1.60333333333334,6.25182190964724E-16,0.));
#8683=CARTESIAN_POINT('',(1.85,4.13736479362129,-5.06681055141326E-16));
#8684=CARTESIAN_POINT('Origin',(1.85,6.70494122533176E-16,0.));
#8685=CARTESIAN_POINT('',(1.60333333333334,4.27977786002139,-5.2412162573369E-16));
#8686=CARTESIAN_POINT('Origin',(1.85,4.14313829631318,0.));
#8687=CARTESIAN_POINT('Origin',(1.54333333333334,4.58,0.));
#8688=CARTESIAN_POINT('Origin',(1.80333333333334,4.29071796769724,0.));
#8689=CARTESIAN_POINT('Origin',(1.64333333333334,4.58,0.));
#8690=CARTESIAN_POINT('Origin',(1.95,4.14313829631318,0.));
#8691=CARTESIAN_POINT('Origin',(1.8,0.,0.));
#8692=CARTESIAN_POINT('',(-1.95,3.2,3.91886975727153E-16));
#8693=CARTESIAN_POINT('Origin',(-1.95,6.88863824520387E-16,0.));
#8694=CARTESIAN_POINT('',(-1.85,3.2,3.91886975727153E-16));
#8695=CARTESIAN_POINT('',(1.8,3.2,3.91886975727153E-16));
#8696=CARTESIAN_POINT('Origin',(-1.85,6.70494122533176E-16,0.));
#8697=CARTESIAN_POINT('Origin',(-1.86,8.67361737988404E-16,0.));
#8698=CARTESIAN_POINT('',(-1.905,4.22108058265378,5.16933282449E-16));
#8699=CARTESIAN_POINT('Origin',(-1.905,6.80597458626142E-16,0.));
#8700=CARTESIAN_POINT('',(-1.95,4.14313829631318,5.07388105300476E-16));
#8701=CARTESIAN_POINT('Origin',(-1.86,4.14313829631318,5.07388105300475E-16));
#8702=CARTESIAN_POINT('Origin',(-1.95,6.88863824520387E-16,0.));
#8703=CARTESIAN_POINT('Origin',(-1.65333333333334,6.34367041958329E-16,
0.));
#8704=CARTESIAN_POINT('',(-1.65333333333334,4.36638040039984,5.3472737812094E-16));
#8705=CARTESIAN_POINT('Origin',(-1.65333333333334,6.34367041958329E-16,
0.));
#8706=CARTESIAN_POINT('',(-1.65333333333334,4.36638040039984,5.3472737812094E-16));
#8707=CARTESIAN_POINT('Origin',(-1.66333333333334,8.67361737988404E-16,
0.));
#8708=CARTESIAN_POINT('',(-1.64333333333333,4.38370090847553,5.3684852859839E-16));
#8709=CARTESIAN_POINT('Origin',(-1.64333333333334,6.32530071759608E-16,
0.));
#8710=CARTESIAN_POINT('Origin',(-1.66333333333334,4.38370090847553,5.3684852859839E-16));
#8711=CARTESIAN_POINT('Origin',(-1.76333333333333,8.67361737988404E-16,
0.));
#8712=CARTESIAN_POINT('',(-1.86725638178747,4.64,5.68236114804372E-16));
#8713=CARTESIAN_POINT('Origin',(-1.86725638178747,6.73664068441309E-16,
0.));
#8714=CARTESIAN_POINT('',(-1.64333333333333,4.58,5.60888234009488E-16));
#8715=CARTESIAN_POINT('Origin',(-1.76333333333333,4.58,5.60888234009488E-16));
#8716=CARTESIAN_POINT('Origin',(-1.64333333333334,6.32530071759608E-16,
0.));
#8717=CARTESIAN_POINT('Origin',(-1.90725638178747,6.81011949236193E-16,
0.));
#8718=CARTESIAN_POINT('',(-1.90725638178747,4.57071796769724,5.59751512894572E-16));
#8719=CARTESIAN_POINT('Origin',(-1.90725638178747,6.81011949236193E-16,
0.));
#8720=CARTESIAN_POINT('',(-1.90725638178747,4.57071796769724,5.59751512894572E-16));
#8721=CARTESIAN_POINT('Origin',(-1.80333333333334,8.67361737988404E-16,
0.));
#8722=CARTESIAN_POINT('',(-1.80333333333334,4.39071796769724,5.3770787050992E-16));
#8723=CARTESIAN_POINT('Origin',(-1.80333333333334,6.61921594939145E-16,
0.));
#8724=CARTESIAN_POINT('Origin',(-1.80333333333334,4.51071796769724,5.52403632099688E-16));
#8725=CARTESIAN_POINT('Origin',(-1.80333333333334,8.67361737988404E-16,
0.));
#8726=CARTESIAN_POINT('',(-1.99385892216591,4.62071796769724,5.65874746890309E-16));
#8727=CARTESIAN_POINT('Origin',(-1.99385892216591,6.96920577817067E-16,
0.));
#8728=CARTESIAN_POINT('',(-1.80333333333334,4.29071796769724,5.25461402518447E-16));
#8729=CARTESIAN_POINT('Origin',(-1.80333333333334,4.51071796769724,5.52403632099688E-16));
#8730=CARTESIAN_POINT('Origin',(-1.80333333333334,6.61921594939145E-16,
0.));
#8731=CARTESIAN_POINT('Origin',(-1.99385892216591,6.96920577817067E-16,
0.));
#8732=CARTESIAN_POINT('',(-1.95385892216591,4.69,5.74359348800109E-16));
#8733=CARTESIAN_POINT('Origin',(-1.95385892216591,6.89572697022182E-16,
0.));
#8734=CARTESIAN_POINT('',(-1.99385892216591,4.62071796769724,5.65874746890309E-16));
#8735=CARTESIAN_POINT('Origin',(-1.76333333333333,8.67361737988404E-16,
0.));
#8736=CARTESIAN_POINT('',(-1.54333333333334,4.58,5.60888234009488E-16));
#8737=CARTESIAN_POINT('Origin',(-1.54333333333334,6.14160369772398E-16,
0.));
#8738=CARTESIAN_POINT('Origin',(-1.76333333333333,4.58,5.60888234009488E-16));
#8739=CARTESIAN_POINT('Origin',(-1.66333333333334,8.67361737988404E-16,
0.));
#8740=CARTESIAN_POINT('',(-1.60333333333334,4.27977786002139,5.24121625733691E-16));
#8741=CARTESIAN_POINT('Origin',(-1.60333333333334,6.25182190964724E-16,
0.));
#8742=CARTESIAN_POINT('',(-1.54333333333333,4.38370090847553,5.3684852859839E-16));
#8743=CARTESIAN_POINT('Origin',(-1.66333333333334,4.38370090847553,5.3684852859839E-16));
#8744=CARTESIAN_POINT('Origin',(-1.54333333333334,6.14160369772398E-16,
0.));
#8745=CARTESIAN_POINT('Origin',(-1.60333333333334,6.25182190964724E-16,
0.));
#8746=CARTESIAN_POINT('',(-1.85,4.13736479362129,5.06681055141326E-16));
#8747=CARTESIAN_POINT('Origin',(-1.85,6.70494122533176E-16,0.));
#8748=CARTESIAN_POINT('',(-1.60333333333334,4.27977786002139,5.2412162573369E-16));
#8749=CARTESIAN_POINT('Origin',(-1.85,4.14313829631318,0.));
#8750=CARTESIAN_POINT('Origin',(-1.54333333333334,4.58,0.));
#8751=CARTESIAN_POINT('Origin',(-1.80333333333334,4.29071796769724,0.));
#8752=CARTESIAN_POINT('Origin',(-1.64333333333334,4.58,0.));
#8753=CARTESIAN_POINT('Origin',(-1.95,4.14313829631318,0.));
#8754=CARTESIAN_POINT('',(1.02140518265514E-14,-4.,92.461739559435));
#8755=CARTESIAN_POINT('',(0.,0.,0.));
#8756=CARTESIAN_POINT('',(0.,0.,0.));
#8757=CARTESIAN_POINT('',(0.,0.,0.));
#8758=CARTESIAN_POINT('',(0.,0.,0.));
#8759=CARTESIAN_POINT('',(0.,0.,0.));
#8760=CARTESIAN_POINT('',(0.,0.,0.));
#8761=CARTESIAN_POINT('',(6.84905562031929E-16,-4.,48.6364583401654));
#8762=UNCERTAINTY_MEASURE_WITH_UNIT(LENGTH_MEASURE(0.01),#8780,
'DISTANCE_ACCURACY_VALUE',
'Maximum model space distance between geometric entities at asserted c
onnectivities');
#8763=UNCERTAINTY_MEASURE_WITH_UNIT(LENGTH_MEASURE(0.01),#8780,
'DISTANCE_ACCURACY_VALUE',
'Maximum model space distance between geometric entities at asserted c
onnectivities');
#8764=UNCERTAINTY_MEASURE_WITH_UNIT(LENGTH_MEASURE(0.01),#8780,
'DISTANCE_ACCURACY_VALUE',
'Maximum model space distance between geometric entities at asserted c
onnectivities');
#8765=UNCERTAINTY_MEASURE_WITH_UNIT(LENGTH_MEASURE(0.01),#8780,
'DISTANCE_ACCURACY_VALUE',
'Maximum model space distance between geometric entities at asserted c
onnectivities');
#8766=UNCERTAINTY_MEASURE_WITH_UNIT(LENGTH_MEASURE(0.01),#8780,
'DISTANCE_ACCURACY_VALUE',
'Maximum model space distance between geometric entities at asserted c
onnectivities');
#8767=UNCERTAINTY_MEASURE_WITH_UNIT(LENGTH_MEASURE(0.01),#8780,
'DISTANCE_ACCURACY_VALUE',
'Maximum model space distance between geometric entities at asserted c
onnectivities');
#8768=UNCERTAINTY_MEASURE_WITH_UNIT(LENGTH_MEASURE(0.01),#8780,
'DISTANCE_ACCURACY_VALUE',
'Maximum model space distance between geometric entities at asserted c
onnectivities');
#8769=UNCERTAINTY_MEASURE_WITH_UNIT(LENGTH_MEASURE(0.01),#8780,
'DISTANCE_ACCURACY_VALUE',
'Maximum model space distance between geometric entities at asserted c
onnectivities');
#8770=UNCERTAINTY_MEASURE_WITH_UNIT(LENGTH_MEASURE(0.01),#8780,
'DISTANCE_ACCURACY_VALUE',
'Maximum model space distance between geometric entities at asserted c
onnectivities');
#8771=(
GEOMETRIC_REPRESENTATION_CONTEXT(3)
GLOBAL_UNCERTAINTY_ASSIGNED_CONTEXT((#8762))
GLOBAL_UNIT_ASSIGNED_CONTEXT((#8780,#8782,#8783))
REPRESENTATION_CONTEXT('','3D')
);
#8772=(
GEOMETRIC_REPRESENTATION_CONTEXT(3)
GLOBAL_UNCERTAINTY_ASSIGNED_CONTEXT((#8763))
GLOBAL_UNIT_ASSIGNED_CONTEXT((#8780,#8782,#8783))
REPRESENTATION_CONTEXT('','3D')
);
#8773=(
GEOMETRIC_REPRESENTATION_CONTEXT(3)
GLOBAL_UNCERTAINTY_ASSIGNED_CONTEXT((#8764))
GLOBAL_UNIT_ASSIGNED_CONTEXT((#8780,#8782,#8783))
REPRESENTATION_CONTEXT('','3D')
);
#8774=(
GEOMETRIC_REPRESENTATION_CONTEXT(3)
GLOBAL_UNCERTAINTY_ASSIGNED_CONTEXT((#8765))
GLOBAL_UNIT_ASSIGNED_CONTEXT((#8780,#8782,#8783))
REPRESENTATION_CONTEXT('','3D')
);
#8775=(
GEOMETRIC_REPRESENTATION_CONTEXT(3)
GLOBAL_UNCERTAINTY_ASSIGNED_CONTEXT((#8766))
GLOBAL_UNIT_ASSIGNED_CONTEXT((#8780,#8782,#8783))
REPRESENTATION_CONTEXT('','3D')
);
#8776=(
GEOMETRIC_REPRESENTATION_CONTEXT(3)
GLOBAL_UNCERTAINTY_ASSIGNED_CONTEXT((#8767))
GLOBAL_UNIT_ASSIGNED_CONTEXT((#8780,#8782,#8783))
REPRESENTATION_CONTEXT('','3D')
);
#8777=(
GEOMETRIC_REPRESENTATION_CONTEXT(3)
GLOBAL_UNCERTAINTY_ASSIGNED_CONTEXT((#8768))
GLOBAL_UNIT_ASSIGNED_CONTEXT((#8780,#8782,#8783))
REPRESENTATION_CONTEXT('','3D')
);
#8778=(
GEOMETRIC_REPRESENTATION_CONTEXT(3)
GLOBAL_UNCERTAINTY_ASSIGNED_CONTEXT((#8769))
GLOBAL_UNIT_ASSIGNED_CONTEXT((#8780,#8782,#8783))
REPRESENTATION_CONTEXT('','3D')
);
#8779=(
GEOMETRIC_REPRESENTATION_CONTEXT(3)
GLOBAL_UNCERTAINTY_ASSIGNED_CONTEXT((#8770))
GLOBAL_UNIT_ASSIGNED_CONTEXT((#8780,#8782,#8783))
REPRESENTATION_CONTEXT('','3D')
);
#8780=(
LENGTH_UNIT()
NAMED_UNIT(*)
SI_UNIT(.MILLI.,.METRE.)
);
#8781=(
LENGTH_UNIT()
NAMED_UNIT(*)
SI_UNIT($,.METRE.)
);
#8782=(
NAMED_UNIT(*)
PLANE_ANGLE_UNIT()
SI_UNIT($,.RADIAN.)
);
#8783=(
NAMED_UNIT(*)
SI_UNIT($,.STERADIAN.)
SOLID_ANGLE_UNIT()
);
#8784=SHAPE_DEFINITION_REPRESENTATION(#8792,#8808);
#8785=SHAPE_DEFINITION_REPRESENTATION(#8793,#8809);
#8786=SHAPE_DEFINITION_REPRESENTATION(#8794,#8810);
#8787=SHAPE_DEFINITION_REPRESENTATION(#8795,#8811);
#8788=SHAPE_DEFINITION_REPRESENTATION(#8796,#8812);
#8789=SHAPE_DEFINITION_REPRESENTATION(#8797,#8813);
#8790=SHAPE_DEFINITION_REPRESENTATION(#8798,#8814);
#8791=SHAPE_DEFINITION_REPRESENTATION(#8799,#8815);
#8792=PRODUCT_DEFINITION_SHAPE('',$,#8817);
#8793=PRODUCT_DEFINITION_SHAPE('',$,#8818);
#8794=PRODUCT_DEFINITION_SHAPE('',$,#8819);
#8795=PRODUCT_DEFINITION_SHAPE('',$,#8820);
#8796=PRODUCT_DEFINITION_SHAPE('',$,#8821);
#8797=PRODUCT_DEFINITION_SHAPE('',$,#8822);
#8798=PRODUCT_DEFINITION_SHAPE('',$,#8823);
#8799=PRODUCT_DEFINITION_SHAPE('',$,#8824);
#8800=PRODUCT_DEFINITION_SHAPE($,$,#35);
#8801=PRODUCT_DEFINITION_SHAPE($,$,#36);
#8802=PRODUCT_DEFINITION_SHAPE($,$,#37);
#8803=PRODUCT_DEFINITION_SHAPE($,$,#38);
#8804=PRODUCT_DEFINITION_SHAPE($,$,#39);
#8805=PRODUCT_DEFINITION_SHAPE($,$,#40);
#8806=PRODUCT_DEFINITION_SHAPE($,$,#41);
#8807=PRODUCT_DEFINITION_SHAPE($,$,#42);
#8808=SHAPE_REPRESENTATION('',(#5202,#5714,#5715,#5716,#5717,#5718,#5719,
#5720,#5721),#8771);
#8809=SHAPE_REPRESENTATION('',(#5203),#8772);
#8810=SHAPE_REPRESENTATION('',(#5509),#8773);
#8811=SHAPE_REPRESENTATION('',(#5519),#8774);
#8812=SHAPE_REPRESENTATION('',(#5540),#8775);
#8813=SHAPE_REPRESENTATION('',(#5546),#8776);
#8814=SHAPE_REPRESENTATION('',(#5565),#8777);
#8815=SHAPE_REPRESENTATION('',(#5571),#8778);
#8816=PRODUCT_DEFINITION_CONTEXT('part definition',#8842,'design');
#8817=PRODUCT_DEFINITION('BR-058','BR-058',#8825,#8816);
#8818=PRODUCT_DEFINITION('Wheel','Wheel',#8826,#8816);
#8819=PRODUCT_DEFINITION('Bar','Bar',#8827,#8816);
#8820=PRODUCT_DEFINITION('Arm','Arm',#8828,#8816);
#8821=PRODUCT_DEFINITION('Pin_01','Pin_01',#8829,#8816);
#8822=PRODUCT_DEFINITION('Screw','Screw',#8830,#8816);
#8823=PRODUCT_DEFINITION('Pin_02','Pin_02',#8831,#8816);
#8824=PRODUCT_DEFINITION('Bearing_01','Bearing_01',#8832,#8816);
#8825=PRODUCT_DEFINITION_FORMATION('',$,#8844);
#8826=PRODUCT_DEFINITION_FORMATION('',$,#8845);
#8827=PRODUCT_DEFINITION_FORMATION('',$,#8846);
#8828=PRODUCT_DEFINITION_FORMATION('',$,#8847);
#8829=PRODUCT_DEFINITION_FORMATION('',$,#8848);
#8830=PRODUCT_DEFINITION_FORMATION('',$,#8849);
#8831=PRODUCT_DEFINITION_FORMATION('',$,#8850);
#8832=PRODUCT_DEFINITION_FORMATION('',$,#8851);
#8833=PRODUCT_RELATED_PRODUCT_CATEGORY('BR-058','BR-058',(#8844));
#8834=PRODUCT_RELATED_PRODUCT_CATEGORY('Wheel','Wheel',(#8845));
#8835=PRODUCT_RELATED_PRODUCT_CATEGORY('Bar','Bar',(#8846));
#8836=PRODUCT_RELATED_PRODUCT_CATEGORY('Arm','Arm',(#8847));
#8837=PRODUCT_RELATED_PRODUCT_CATEGORY('Pin_01','Pin_01',(#8848));
#8838=PRODUCT_RELATED_PRODUCT_CATEGORY('Screw','Screw',(#8849));
#8839=PRODUCT_RELATED_PRODUCT_CATEGORY('Pin_02','Pin_02',(#8850));
#8840=PRODUCT_RELATED_PRODUCT_CATEGORY('Bearing_01','Bearing_01',(#8851));
#8841=APPLICATION_PROTOCOL_DEFINITION('international standard',
'automotive_design',2009,#8842);
#8842=APPLICATION_CONTEXT(
'Core Data for Automotive Mechanical Design Process');
#8843=PRODUCT_CONTEXT('part definition',#8842,'mechanical');
#8844=PRODUCT('BR-058','BR-058',$,(#8843));
#8845=PRODUCT('Wheel','Wheel',$,(#8843));
#8846=PRODUCT('Bar','Bar',$,(#8843));
#8847=PRODUCT('Arm','Arm',$,(#8843));
#8848=PRODUCT('Pin_01','Pin_01',$,(#8843));
#8849=PRODUCT('Screw','Screw',$,(#8843));
#8850=PRODUCT('Pin_02','Pin_02',$,(#8843));
#8851=PRODUCT('Bearing_01','Bearing_01',$,(#8843));
#8852=PRESENTATION_STYLE_ASSIGNMENT((#8857));
#8853=PRESENTATION_STYLE_ASSIGNMENT((#8858));
#8854=PRESENTATION_STYLE_ASSIGNMENT((#8859));
#8855=PRESENTATION_STYLE_ASSIGNMENT((#8860));
#8856=PRESENTATION_STYLE_ASSIGNMENT((#8861));
#8857=SURFACE_STYLE_USAGE(.BOTH.,#8862);
#8858=SURFACE_STYLE_USAGE(.BOTH.,#8863);
#8859=SURFACE_STYLE_USAGE(.BOTH.,#8864);
#8860=SURFACE_STYLE_USAGE(.BOTH.,#8865);
#8861=SURFACE_STYLE_USAGE(.BOTH.,#8866);
#8862=SURFACE_SIDE_STYLE('',(#8867));
#8863=SURFACE_SIDE_STYLE('',(#8868));
#8864=SURFACE_SIDE_STYLE('',(#8869));
#8865=SURFACE_SIDE_STYLE('',(#8870));
#8866=SURFACE_SIDE_STYLE('',(#8871));
#8867=SURFACE_STYLE_FILL_AREA(#8872);
#8868=SURFACE_STYLE_FILL_AREA(#8873);
#8869=SURFACE_STYLE_FILL_AREA(#8874);
#8870=SURFACE_STYLE_FILL_AREA(#8875);
#8871=SURFACE_STYLE_FILL_AREA(#8876);
#8872=FILL_AREA_STYLE('Steel - Satin',(#8877));
#8873=FILL_AREA_STYLE('Opaque(170,85,255)',(#8878));
#8874=FILL_AREA_STYLE('Opaque(85,170,0)',(#8879));
#8875=FILL_AREA_STYLE('Opaque(85,255,0)',(#8880));
#8876=FILL_AREA_STYLE('Opaque(160,160,160)',(#8881));
#8877=FILL_AREA_STYLE_COLOUR('Steel - Satin',#8882);
#8878=FILL_AREA_STYLE_COLOUR('Opaque(170,85,255)',#8883);
#8879=FILL_AREA_STYLE_COLOUR('Opaque(85,170,0)',#8884);
#8880=FILL_AREA_STYLE_COLOUR('Opaque(85,255,0)',#8885);
#8881=FILL_AREA_STYLE_COLOUR('Opaque(160,160,160)',#8886);
#8882=COLOUR_RGB('Steel - Satin', 0.09019608, 0.27058824, 0.51372549);
#8883=COLOUR_RGB('Opaque(170,85,255)', 0.09019608, 0.27058824, 0.51372549);
#8884=COLOUR_RGB('Opaque(85,170,0)', 0.66274510, 0.83137255, 0.94901961);
#8885=COLOUR_RGB('Opaque(85,255,0)', 0.31764706, 0.68627451, 0.89019608);
#8886=COLOUR_RGB('Opaque(160,160,160)', 0.72549020, 0.75294118, 0.79215686);
ENDSEC;
END-ISO-10303-21;
